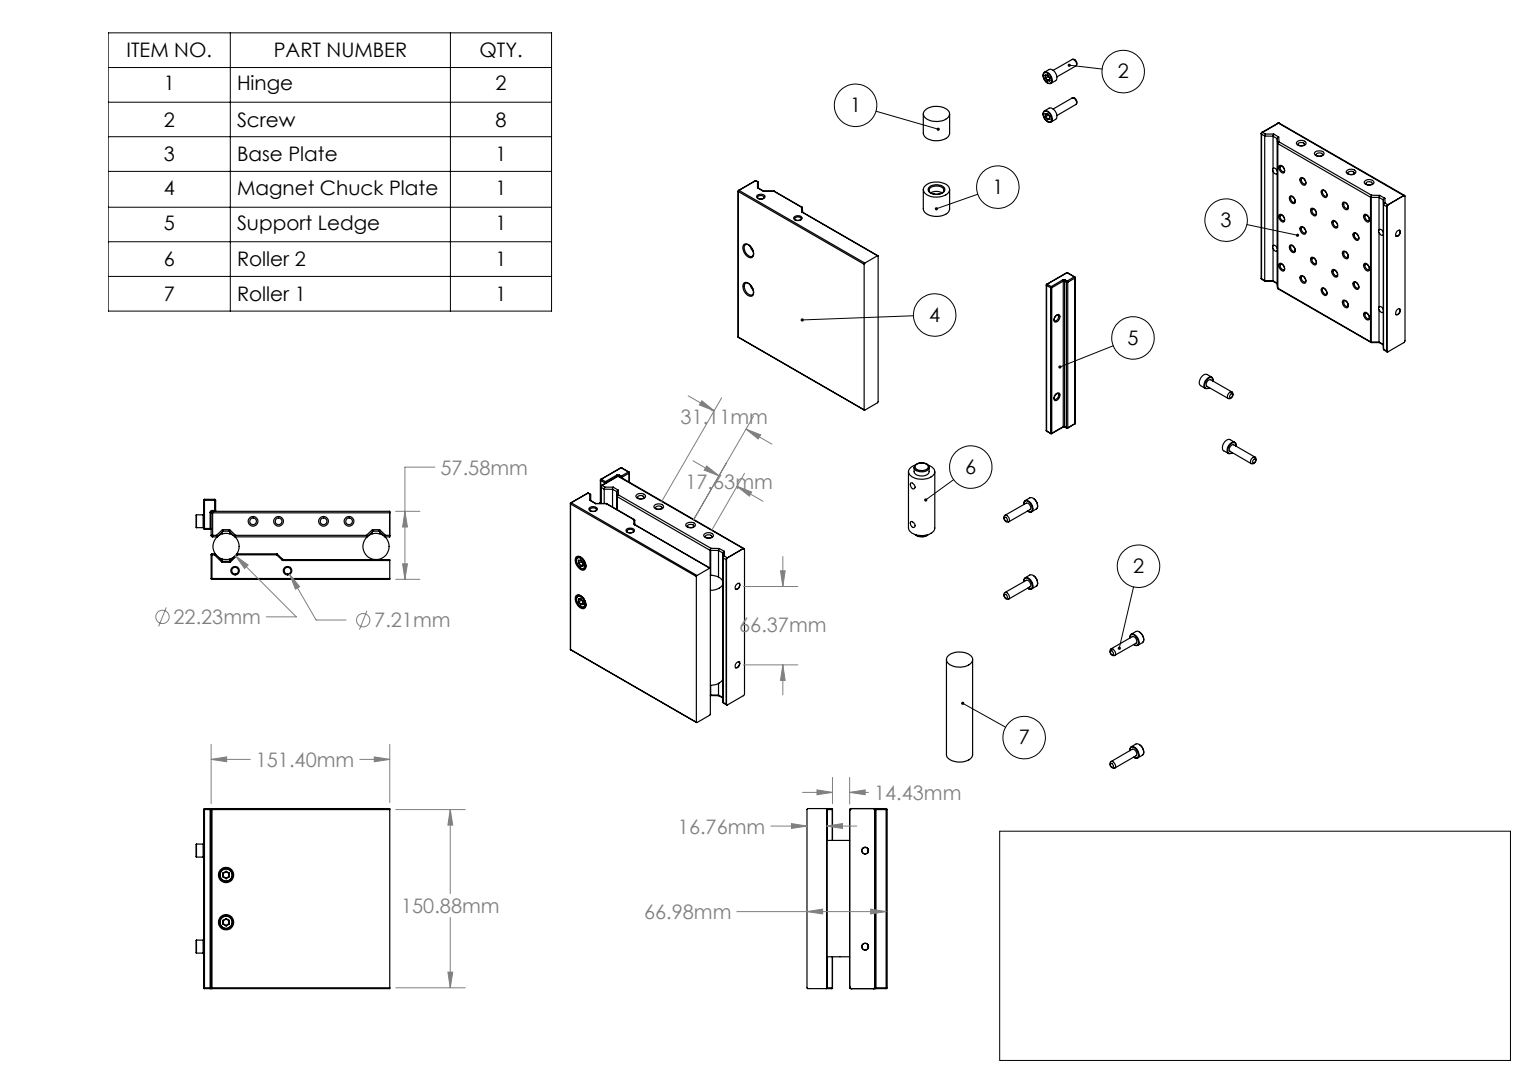
ISO-10303-21;
HEADER;
FILE_DESCRIPTION (('STEP AP214'),
    '1' );
FILE_NAME ('MAT-035',
    '2026-10-26T17:37:43',
    ( '' ),
    ( '' ),
    'SwSTEP 2.0',
    'SolidWorks 2024',
    '' );
FILE_SCHEMA (( 'AUTOMOTIVE_DESIGN' ));
ENDSEC;

DATA;
#1 = EDGE_CURVE ( 'NONE', #5531, #18286, #22565, .T. ) ;
#2 = CARTESIAN_POINT ( 'NONE',  ( 137.0307011298872908, -3580.478779010893959, 2249.731360258177119 ) ) ;
#3 = EDGE_LOOP ( 'NONE', ( #5328, #3633, #22102, #2471 ) ) ;
#4 = DIRECTION ( 'NONE',  ( 0.000000000000000000, 1.000000000000000000, 0.000000000000000000 ) ) ;
#5 = DATE_AND_TIME ( #19692, #20234 ) ;
#6 = CARTESIAN_POINT ( 'NONE',  ( 12.69999999999999929, -3585.971999999999753, 2263.117139999999836 ) ) ;
#7 = CARTESIAN_POINT ( 'NONE',  ( 116.8400000000000034, -3543.299999999999727, 2247.392000000000280 ) ) ;
#8 = VECTOR ( 'NONE', #2227, 1000.000000000000000 ) ;
#9 = DIRECTION ( 'NONE',  ( -1.000000000000000000, 0.000000000000000000, 0.000000000000000000 ) ) ;
#10 = CARTESIAN_POINT ( 'NONE',  ( 0.7620000000000000107, -3544.061999999999898, 2275.763800000000174 ) ) ;
#11 = LOCAL_TIME ( 17, 37, 43.00000000000000000, #12683 ) ;
#12 = CARTESIAN_POINT ( 'NONE',  ( 17.78000000000000114, -3579.494999999999891, 2239.009999999999764 ) ) ;
#13 = EDGE_LOOP ( 'NONE', ( #4801, #14751 ) ) ;
#14 = AXIS2_PLACEMENT_3D ( 'NONE', #15354, #18865, #22602 ) ;
#15 = CARTESIAN_POINT ( 'NONE',  ( 15.55036781974841453, -3695.600514565457615, 2254.996746371283280 ) ) ;
#16 = FACE_OUTER_BOUND ( 'NONE', #5974, .T. ) ;
#17 = ORIENTED_EDGE ( 'NONE', *, *, #15739, .F. ) ;
#18 = CARTESIAN_POINT ( 'NONE',  ( 50.79999999999999716, -3619.500000000000000, 2259.837999999999738 ) ) ;
#19 = LINE ( 'NONE', #12552, #15858 ) ;
#20 = DIRECTION ( 'NONE',  ( 9.756599977372053330E-14, 0.000000000000000000, -1.000000000000000000 ) ) ;
#21 = ORIENTED_EDGE ( 'NONE', *, *, #16592, .T. ) ;
#22 = FACE_OUTER_BOUND ( 'NONE', #22533, .T. ) ;
#23 = DIRECTION ( 'NONE',  ( 0.000000000000000000, 0.000000000000000000, -1.000000000000000000 ) ) ;
#24 = ORIENTED_EDGE ( 'NONE', *, *, #21540, .F. ) ;
#25 = DIRECTION ( 'NONE',  ( 1.000000000000000000, 0.000000000000000000, 3.996303350731721563E-14 ) ) ;
#26 = CARTESIAN_POINT ( 'NONE',  ( 11.76763247656000111, -3642.196447741000156, 2279.779831143999672 ) ) ;
#27 =( NAMED_UNIT ( * ) SI_UNIT ( $, .STERADIAN. ) SOLID_ANGLE_UNIT ( ) );
#28 = SECURITY_CLASSIFICATION ( '', '', #9371 ) ;
#29 = CARTESIAN_POINT ( 'NONE',  ( 17.55427699106284933, -3576.478798487876247, 2245.835327951717773 ) ) ;
#30 = APPLIED_APPROVAL_ASSIGNMENT ( #2619, ( #10933 ) ) ;
#31 = DIRECTION ( 'NONE',  ( 0.000000000000000000, 0.000000000000000000, -1.000000000000000000 ) ) ;
#32 = DATE_AND_TIME ( #21248, #20949 ) ;
#33 = CARTESIAN_POINT ( 'NONE',  ( 139.6999999999999886, -3574.034000000000106, 2239.391000000000076 ) ) ;
#34 = CARTESIAN_POINT ( 'NONE',  ( 9.652920519510999497, -3695.699999999999818, 2254.503999999999905 ) ) ;
#35 = ORIENTED_EDGE ( 'NONE', *, *, #2844, .F. ) ;
#36 = DIRECTION ( 'NONE',  ( 0.000000000000000000, 0.000000000000000000, -1.000000000000000000 ) ) ;
#37 = CARTESIAN_POINT ( 'NONE',  ( 137.2900278743959745, -3657.993505329751770, 2249.258937114173477 ) ) ;
#38 = ORIENTED_EDGE ( 'NONE', *, *, #8360, .F. ) ;
#39 = PLANE ( 'NONE',  #20096 ) ;
#40 = APPLIED_PERSON_AND_ORGANIZATION_ASSIGNMENT ( #1758, #22954, ( #741 ) ) ;
#41 = ORIENTED_EDGE ( 'NONE', *, *, #19227, .F. ) ;
#42 = EDGE_LOOP ( 'NONE', ( #2703, #1001, #9067, #21720 ) ) ;
#43 = SECURITY_CLASSIFICATION ( '', '', #12160 ) ;
#44 = LOCAL_TIME ( 17, 37, 43.00000000000000000, #19509 ) ;
#45 = EDGE_LOOP ( 'NONE', ( #8949, #290, #14111, #10584 ) ) ;
#46 = DIRECTION ( 'NONE',  ( 0.000000000000000000, 0.000000000000000000, -1.000000000000000000 ) ) ;
#47 = EDGE_CURVE ( 'NONE', #7611, #9417, #20192, .T. ) ;
#48 = ORIENTED_EDGE ( 'NONE', *, *, #14973, .T. ) ;
#49 = ORIENTED_EDGE ( 'NONE', *, *, #4852, .F. ) ;
#50 = DIRECTION ( 'NONE',  ( 0.000000000000000000, 0.000000000000000000, -1.000000000000000000 ) ) ;
#51 = ADVANCED_FACE ( 'NONE', ( #16778 ), #19588, .T. ) ;
#52 = APPROVAL_STATUS ( 'not_yet_approved' ) ;
#53 = LINE ( 'NONE', #7432, #17005 ) ;
#54 = CYLINDRICAL_SURFACE ( 'NONE', #7821, 5.714999999999998082 ) ;
#55 = EDGE_CURVE ( 'NONE', #4791, #12834, #15371, .T. ) ;
#56 = EDGE_LOOP ( 'NONE', ( #1910, #7184, #18432, #2575 ) ) ;
#57 = AXIS2_PLACEMENT_3D ( 'NONE', #16806, #751, #19035 ) ;
#58 = CARTESIAN_POINT ( 'NONE',  ( 12.69999999999999929, -3579.494999999999891, 2246.630000000000109 ) ) ;
#59 = CYLINDRICAL_SURFACE ( 'NONE', #10460, 2.844800000000091700 ) ;
#60 = CARTESIAN_POINT ( 'NONE',  ( -12.31900000000000084, -3660.140000000000327, 2247.392000000000280 ) ) ;
#61 = CARTESIAN_POINT ( 'NONE',  ( 116.8400000000000034, -3694.430000000000291, 2247.392000000000280 ) ) ;
#62 = APPROVAL_DATE_TIME ( #1579, #4060 ) ;
#63 = EDGE_CURVE ( 'NONE', #17851, #18027, #1534, .T. ) ;
#64 = DIRECTION ( 'NONE',  ( 0.000000000000000000, -2.336881798971000105E-14, 1.000000000000000000 ) ) ;
#65 = ORIENTED_EDGE ( 'NONE', *, *, #14589, .T. ) ;
#66 = CARTESIAN_POINT ( 'NONE',  ( 9.987313202991684236, -3657.938829547518253, 2239.009999999999764 ) ) ;
#67 = DIRECTION ( 'NONE',  ( 0.000000000000000000, 0.000000000000000000, 1.000000000000000000 ) ) ;
#68 = ORIENTED_EDGE ( 'NONE', *, *, #2483, .T. ) ;
#69 = AXIS2_PLACEMENT_3D ( 'NONE', #21536, #19655, #7123 ) ;
#70 = DIRECTION ( 'NONE',  ( -1.000000000000000000, 2.330758767201999921E-14, 2.343004830739999973E-14 ) ) ;
#71 = CARTESIAN_POINT ( 'NONE',  ( 25.39999999999999858, -3660.140000000000327, 2247.392000000000280 ) ) ;
#72 = CARTESIAN_POINT ( 'NONE',  ( 41.70680000000000121, -3644.899999999999636, 2239.009999999999764 ) ) ;
#73 = CARTESIAN_POINT ( 'NONE',  ( 151.1299999999999955, -3694.430000000000291, 2259.329999999999927 ) ) ;
#74 = DIRECTION ( 'NONE',  ( 0.000000000000000000, 0.000000000000000000, 1.000000000000000000 ) ) ;
#75 = CARTESIAN_POINT ( 'NONE',  ( 18.25500259602790720, -3658.162202898845862, 2245.347138497373180 ) ) ;
#76 = EDGE_CURVE ( 'NONE', #7743, #14640, #1242, .T. ) ;
#77 = EDGE_LOOP ( 'NONE', ( #5442, #11222, #19525, #6801 ) ) ;
#78 = FACE_OUTER_BOUND ( 'NONE', #21782, .T. ) ;
#79 = EDGE_CURVE ( 'NONE', #18611, #6224, #7995, .T. ) ;
#80 = DIRECTION ( 'NONE',  ( 0.000000000000000000, 0.000000000000000000, 1.000000000000000000 ) ) ;
#81 = EDGE_CURVE ( 'NONE', #2498, #2000, #21462, .T. ) ;
#82 = LINE ( 'NONE', #12499, #17173 ) ;
#83 = DIRECTION ( 'NONE',  ( -5.461016542361937364E-28, 1.000000000000000000, -2.336881798971000105E-14 ) ) ;
#84 = CARTESIAN_POINT ( 'NONE',  ( 137.1117535491106594, -3694.976217804482530, 2255.653245237783267 ) ) ;
#85 = ORIENTED_EDGE ( 'NONE', *, *, #8808, .F. ) ;
#86 = AXIS2_PLACEMENT_3D ( 'NONE', #9991, #1078, #11873 ) ;
#87 = DIRECTION ( 'NONE',  ( 0.000000000000000000, 0.000000000000000000, 1.000000000000000000 ) ) ;
#88 = ORIENTED_EDGE ( 'NONE', *, *, #6716, .T. ) ;
#89 = AXIS2_PLACEMENT_3D ( 'NONE', #13714, #3272, #12061 ) ;
#90 = DIRECTION ( 'NONE',  ( 1.000000000000000000, 0.000000000000000000, 0.000000000000000000 ) ) ;
#91 = CARTESIAN_POINT ( 'NONE',  ( 135.0886139726000010, -3662.880847139000252, 2246.630000000000109 ) ) ;
#92 = CALENDAR_DATE ( 2026, 26, 10 ) ;
#93 = CYLINDRICAL_SURFACE ( 'NONE', #6462, 1.269999999999882334 ) ;
#94 = CARTESIAN_POINT ( 'NONE',  ( 3.048000000000000043, -3544.061999999999898, 2228.849999999999909 ) ) ;
#95 = DIRECTION ( 'NONE',  ( -2.336881798971000105E-14, 0.000000000000000000, -1.000000000000000000 ) ) ;
#96 = ADVANCED_FACE ( 'NONE', ( #13964 ), #8465, .F. ) ;
#97 = AXIS2_PLACEMENT_3D ( 'NONE', #21852, #23131, #10839 ) ;
#98 = DIRECTION ( 'NONE',  ( 0.000000000000000000, 0.000000000000000000, 1.000000000000000000 ) ) ;
#99 = AXIS2_PLACEMENT_3D ( 'NONE', #19425, #3130, #10398 ) ;
#100 = ORIENTED_EDGE ( 'NONE', *, *, #20293, .T. ) ;
#101 = DIRECTION ( 'NONE',  ( 0.000000000000000000, 0.000000000000000000, 1.000000000000000000 ) ) ;
#102 = ORIENTED_EDGE ( 'NONE', *, *, #7130, .F. ) ;
#103 = TOROIDAL_SURFACE ( 'NONE', #6096, 3.606799999999999784, 0.7620000000000000107 ) ;
#104 = DIRECTION ( 'NONE',  ( 0.000000000000000000, 0.000000000000000000, -1.000000000000000000 ) ) ;
#105 = CIRCLE ( 'NONE', #22163, 3.606799999999993567 ) ;
#106 = CARTESIAN_POINT ( 'NONE',  ( 139.6999999999999886, -3659.504999999999654, 2272.030000000000200 ) ) ;
#107 = ORIENTED_EDGE ( 'NONE', *, *, #21741, .F. ) ;
#108 = CARTESIAN_POINT ( 'NONE',  ( 85.29320000000001301, -3644.899999999999636, 2239.009999999999764 ) ) ;
#109 = B_SPLINE_CURVE_WITH_KNOTS ( 'NONE', 3,
 ( #11658, #15542, #8166, #2887, #6654, #22328, #18938, #6532, #2998, #1356, #1238, #17171, #20933, #8046, #13430, #10031, #13667, #10147, #3112, #15428, #1118, #2762, #4874, #20571, #12026, #4523, #19295, #6764, #17285, #8277, #9904, #15664, #4637, #20688, #8398, #18816, #19176, #8521, #22561, #22681, #20817, #22437, #17053, #1005, #15312, #6412, #19058, #17399, #13905, #11785, #22788, #21052 ),
 .UNSPECIFIED., .F., .F.,
 ( 4, 2, 1, 1, 1, 1, 2, 2, 2, 1, 2, 2, 2, 2, 1, 1, 1, 2, 2, 2, 2, 1, 1, 1, 2, 2, 2, 1, 1, 1, 2, 2, 4 ),
 ( 0.000000000000000000, 0.003906250000015105105, 0.007812500000030210209, 0.01562500000044777723, 0.03125000000089964147, 0.06250000000180337689, 0.1250000000036391445, 0.2500000000076161855, 0.2656250000084233176, 0.2812500000092305052, 0.3125000000108511533, 0.3750000000142236778, 0.5000000000208256745, 0.5019531250208819628, 0.5039062500209382511, 0.5078125000210353956, 0.5156250000208461026, 0.5312500000204676276, 0.5625000000200504058, 0.6250000000192512672, 0.6289062500191696659, 0.6328125000190880645, 0.6406250000187544424, 0.6562500000179013471, 0.6875000000160184088, 0.7500000000124475985, 0.7539062500122738486, 0.7578125000121000987, 0.7656250000119128041, 0.7812500000113792309, 0.8125000000098967501, 0.8750000000066556760, 1.000000000000000000 ),
 .UNSPECIFIED. ) ;
#110 = EDGE_LOOP ( 'NONE', ( #14632, #871, #3105, #5719 ) ) ;
#111 = CARTESIAN_POINT ( 'NONE',  ( 142.6612001523742208, -3695.684722679518018, 2254.718298691088421 ) ) ;
#112 = DIRECTION ( 'NONE',  ( 1.000000000000000000, 0.000000000000000000, 0.000000000000000000 ) ) ;
#113 = AXIS2_PLACEMENT_3D ( 'NONE', #6268, #9537, #4040 ) ;
#114 = ORIENTED_EDGE ( 'NONE', *, *, #1797, .F. ) ;
#115 = EDGE_CURVE ( 'NONE', #4940, #21098, #2726, .T. ) ;
#116 = ADVANCED_FACE ( 'NONE', ( #12202 ), #6711, .T. ) ;
#117 = CARTESIAN_POINT ( 'NONE',  ( 137.1107034105660034, -3580.676250239197998, 2249.584241783140442 ) ) ;
#118 = VERTEX_POINT ( 'NONE', #15723 ) ;
#119 = DIRECTION ( 'NONE',  ( 1.224646799147353207E-16, 1.000000000000000000, -0.000000000000000000 ) ) ;
#120 = APPLICATION_PROTOCOL_DEFINITION ( 'international standard', 'automotive_design', 2000, #14590 ) ;
#121 = CIRCLE ( 'NONE', #1224, 2.844800000000091700 ) ;
#122 = CARTESIAN_POINT ( 'NONE',  ( 6.996782844457664297, -3579.071241691879095, 2244.547217133379945 ) ) ;
#123 = DIRECTION ( 'NONE',  ( 0.000000000000000000, 0.000000000000000000, -1.000000000000000000 ) ) ;
#124 = ADVANCED_FACE ( 'NONE', ( #19237 ), #13848, .F. ) ;
#125 = DIRECTION ( 'NONE',  ( -1.000000000000000000, 0.000000000000000000, 0.000000000000000000 ) ) ;
#126 = CARTESIAN_POINT ( 'NONE',  ( 12.69999999994000106, -3596.805100000000039, 2292.781800000000203 ) ) ;
#127 = EDGE_LOOP ( 'NONE', ( #9464, #14168, #22567, #17753 ) ) ;
#128 = CARTESIAN_POINT ( 'NONE',  ( 141.9735787716368804, -3577.784544496731542, 2250.025932887172985 ) ) ;
#129 = EDGE_LOOP ( 'NONE', ( #9920, #914 ) ) ;
#130 = AXIS2_PLACEMENT_3D ( 'NONE', #3984, #794, #16512 ) ;
#131 = CARTESIAN_POINT ( 'NONE',  ( 134.0223127011804252, -3578.842640279839998, 2244.547249493357413 ) ) ;
#132 = EDGE_CURVE ( 'NONE', #6511, #15378, #5378, .T. ) ;
#133 = EDGE_CURVE ( 'NONE', #17829, #16978, #3861, .T. ) ;
#134 = CARTESIAN_POINT ( 'NONE',  ( 15.49601198374999989, -3578.946622428999945, 2257.950097350999840 ) ) ;
#135 = ORIENTED_EDGE ( 'NONE', *, *, #969, .F. ) ;
#136 = CARTESIAN_POINT ( 'NONE',  ( 9.970491213060000746, -3580.312548418000006, 2257.932969814999979 ) ) ;
#137 = FACE_OUTER_BOUND ( 'NONE', #12525, .T. ) ;
#138 = CIRCLE ( 'NONE', #3486, 0.7619999999999987894 ) ;
#139 = CLOSED_SHELL ( 'NONE', ( #18289, #7008, #8518, #22594, #20989, #23105, #16145, #3413, #11794, #2224, #2827, #1410, #16543, #19416, #8130, #13424, #4558, #15262, #22286, #8396, #19575, #9289, #13963, #21111, #15810, #7255, #18256, #22413, #19334, #8366, #20531, #3559, #5670, #14740, #18979, #14141, #9599, #14263, #10124, #6147, #22178, #12747, #12264, #9427, #21177, #17826, #16370, #12412, #15426, #5281, #20386, #14683, #16750, #2410, #10013, #13395, #16311, #7711, #4641, #19449, #4494, #20415, #21019, #22225, #51, #6503, #13150, #17175, #14109, #16374, #18246, #13592, #4477, #20450, #11729, #3837, #17376, #8709, #18820, #14659, #4694, #4420, #5580, #11076, #2706, #6139, #12300, #1249, #21474, #5517, #12872, #14173, #13268, #987, #12573, #13097, #1664, #18403, #22007, #19391, #3382, #1211, #5961, #11237, #5886, #6240, #19563, #17791, #16108, #12536, #16780, #15034, #22219, #16319, #12028, #639, #4268, #6646, #19581, #19988, #13241, #6285, #15946, #4264, #21207, #2054, #22523, #7877, #11589, #22115, #16270, #96, #13253, #16398, #4808, #22277, #13435, #22678, #11382, #13308, #16585, #7024, #2755, #9237, #5116, #15881, #12312, #7534, #10663, #16517, #6439, #10126, #19876, #16966, #14807, #20512, #21309, #6853, #805, #16656, #19994, #11360, #8292, #8247, #511, #18141, #8217, #8284, #20809, #15008, #18035, #14102, #15702, #2487, #7663, #10088, #14883, #1165, #15813, #6527, #13028, #17258, #14527, #3507, #2757, #21880, #10849, #8534, #17415, #20660, #18719, #3789, #13015, #1704, #22836, #5727, #9542, #18530, #20029, #22101, #3836, #20839, #5077, #16041, #11870, #14827, #21582, #6419, #5871, #17134, #3910, #5590, #14945, #16186, #7678, #21286, #12539, #7356, #7419, #6403, #1767, #10423, #16431, #5343, #124, #22382, #20876, #14160, #2061, #4392, #471, #2508, #9317, #22720, #967, #22838, #18612, #8833, #5095, #23099, #12516, #18309, #6530, #2705, #20259, #5803, #15689, #10375, #23161, #22806, #22870, #9927, #11310, #13967, #17673, #19716, #15974, #22128, #14003, #5885, #23135, #5290, #5119, #11638, #6284, #7996, #769, #4193, #15853, #18569, #4096, #19675, #3268, #9017, #3364, #233, #11495, #6410, #14763, #6092, #8252, #7227, #12142, #21432 ) ) ;
#140 = VERTEX_POINT ( 'NONE', #15613 ) ;
#141 = DIRECTION ( 'NONE',  ( 1.000000000000000000, 0.000000000000000000, 0.000000000000000000 ) ) ;
#142 = DIRECTION ( 'NONE',  ( 0.000000000000000000, 0.000000000000000000, 1.000000000000000000 ) ) ;
#143 = ORIENTED_EDGE ( 'NONE', *, *, #16586, .F. ) ;
#144 = CARTESIAN_POINT ( 'NONE',  ( -12.69999999999999929, -3577.293829546999859, 2244.679313203000220 ) ) ;
#145 = EDGE_CURVE ( 'NONE', #4963, #5906, #6598, .T. ) ;
#146 = CARTESIAN_POINT ( 'NONE',  ( 139.7000000000063835, -3656.812599999938357, 2239.391000000000076 ) ) ;
#147 = CARTESIAN_POINT ( 'NONE',  ( 86.05520000000001346, -3644.899999999999636, 2261.869999999999891 ) ) ;
#148 = CARTESIAN_POINT ( 'NONE',  ( 35.56000000000000227, -3694.430000000000291, 2243.277199999999993 ) ) ;
#149 = CIRCLE ( 'NONE', #19230, 4.114799999999974034 ) ;
#150 = APPROVAL_ROLE ( '' ) ;
#151 = FACE_OUTER_BOUND ( 'NONE', #1516, .T. ) ;
#152 = CARTESIAN_POINT ( 'NONE',  ( 9.823095770001307514, -3695.626565546511301, 2254.929879519301721 ) ) ;
#153 = EDGE_LOOP ( 'NONE', ( #3229, #589, #13779, #13464, #20523, #7090, #21786, #14841 ) ) ;
#154 = CARTESIAN_POINT ( 'NONE',  ( 18.26408956042804377, -3580.799603742805175, 2245.310931594975045 ) ) ;
#155 = CARTESIAN_POINT ( 'NONE',  ( 137.5777489049088160, -3657.610548859369828, 2248.693836209597066 ) ) ;
#156 = ORIENTED_EDGE ( 'NONE', *, *, #8169, .T. ) ;
#157 = ORIENTED_EDGE ( 'NONE', *, *, #22934, .F. ) ;
#158 = CARTESIAN_POINT ( 'NONE',  ( 137.6199768978073905, -3661.447896576730727, 2249.919485654132586 ) ) ;
#159 = VERTEX_POINT ( 'NONE', #14082 ) ;
#160 = ORIENTED_EDGE ( 'NONE', *, *, #9548, .T. ) ;
#161 = ORIENTED_EDGE ( 'NONE', *, *, #12576, .T. ) ;
#162 = AXIS2_PLACEMENT_3D ( 'NONE', #11218, #12637, #3839 ) ;
#163 = DIRECTION ( 'NONE',  ( 0.000000000000000000, 0.000000000000000000, -1.000000000000000000 ) ) ;
#164 = CIRCLE ( 'NONE', #18872, 1.270000000000000018 ) ;
#165 = ORIENTED_EDGE ( 'NONE', *, *, #16586, .T. ) ;
#166 = ORIENTED_EDGE ( 'NONE', *, *, #22581, .T. ) ;
#167 = DIRECTION ( 'NONE',  ( 1.000000000000000000, -0.000000000000000000, -0.000000000000000000 ) ) ;
#168 = CALENDAR_DATE ( 2026, 26, 10 ) ;
#169 = CARTESIAN_POINT ( 'NONE',  ( 9.956800000000452400, -3660.383257047480583, 2255.967039999999997 ) ) ;
#170 = ORIENTED_EDGE ( 'NONE', *, *, #1350, .F. ) ;
#171 = DIRECTION ( 'NONE',  ( 0.000000000000000000, 1.000000000000000000, 0.000000000000000000 ) ) ;
#172 = CARTESIAN_POINT ( 'NONE',  ( 10.36831320293797276, -3578.148799999986750, 2239.391000000000076 ) ) ;
#173 = PLANE ( 'NONE',  #10602 ) ;
#174 = CARTESIAN_POINT ( 'NONE',  ( -8.890000000008001280, -3580.206200000000081, 2249.723686796999573 ) ) ;
#175 = APPROVAL_DATE_TIME ( #17870, #4630 ) ;
#176 = APPROVAL ( #3017, 'UNKNOWN' ) ;
#177 = CARTESIAN_POINT ( 'NONE',  ( 142.5448000000000093, -3579.495004790000166, 2250.165035197999714 ) ) ;
#178 = EDGE_LOOP ( 'NONE', ( #370, #14088 ) ) ;
#179 = AXIS2_PLACEMENT_3D ( 'NONE', #16153, #101, #7252 ) ;
#180 = AXIS2_PLACEMENT_3D ( 'NONE', #4106, #4219, #18284 ) ;
#181 = CARTESIAN_POINT ( 'NONE',  ( 151.1299999999999955, -3544.570000000000164, 2240.279999999999745 ) ) ;
#182 = EDGE_CURVE ( 'NONE', #17917, #2186, #21094, .T. ) ;
#183 = CARTESIAN_POINT ( 'NONE',  ( 7.963520823585933606, -3662.703639150101026, 2246.156481404430906 ) ) ;
#184 = AXIS2_PLACEMENT_3D ( 'NONE', #20222, #9553, #4165 ) ;
#185 = VERTEX_POINT ( 'NONE', #21235 ) ;
#186 = CARTESIAN_POINT ( 'NONE',  ( 139.6999999999999886, -3659.504999999999654, 2239.391000000000076 ) ) ;
#187 = CARTESIAN_POINT ( 'NONE',  ( 9.987313202740898177, -3661.071170452786646, 2239.009999999999764 ) ) ;
#188 = CARTESIAN_POINT ( 'NONE',  ( 139.6999999999999886, -3579.494999999999891, 2239.009999999999764 ) ) ;
#189 = DIRECTION ( 'NONE',  ( 0.000000000000000000, 1.000000000000000000, 0.000000000000000000 ) ) ;
#190 = ORIENTED_EDGE ( 'NONE', *, *, #21850, .F. ) ;
#191 = CARTESIAN_POINT ( 'NONE',  ( 20.32000000000000028, -3568.700000000000273, 2289.213099999999940 ) ) ;
#192 = EDGE_LOOP ( 'NONE', ( #13601, #391, #20890, #19127 ) ) ;
#193 = CARTESIAN_POINT ( 'NONE',  ( 147.4191677002133929, -3695.185487567203381, 2260.351709085013226 ) ) ;
#194 = AXIS2_PLACEMENT_3D ( 'NONE', #19267, #12347, #20783 ) ;
#195 = CARTESIAN_POINT ( 'NONE',  ( 25.39999999999999858, -3670.300000000000182, 2239.771999999999935 ) ) ;
#196 = AXIS2_PLACEMENT_3D ( 'NONE', #17467, #5408, #21233 ) ;
#197 = DIRECTION ( 'NONE',  ( 0.000000000000000000, 0.000000000000000000, -1.000000000000000000 ) ) ;
#198 = AXIS2_PLACEMENT_3D ( 'NONE', #803, #13353, #20498 ) ;
#199 = DIRECTION ( 'NONE',  ( -1.000000000000000000, -3.885294924352999876E-13, 3.885294924352999876E-13 ) ) ;
#200 = CIRCLE ( 'NONE', #6578, 0.7619999999999294005 ) ;
#201 = DIRECTION ( 'NONE',  ( 0.000000000000000000, 0.000000000000000000, -1.000000000000000000 ) ) ;
#202 = DIRECTION ( 'NONE',  ( 0.000000000000000000, 0.000000000000000000, -1.000000000000000000 ) ) ;
#203 = CARTESIAN_POINT ( 'NONE',  ( 7.471656874357363698, -3577.187248168970200, 2245.090911189840881 ) ) ;
#204 = VERTEX_POINT ( 'NONE', #22501 ) ;
#205 = COORDINATED_UNIVERSAL_TIME_OFFSET ( 0, 0, .AHEAD. ) ;
#206 = APPLIED_PERSON_AND_ORGANIZATION_ASSIGNMENT ( #22202, #11540, ( #4495 ) ) ;
#207 = CARTESIAN_POINT ( 'NONE',  ( -6.349999999999999645, -3578.860000000000127, 2250.998800000000301 ) ) ;
#208 = CARTESIAN_POINT ( 'NONE',  ( 64.76999999999999602, -3544.061999999999898, 2285.606299999999919 ) ) ;
#209 = SECURITY_CLASSIFICATION_LEVEL ( 'unclassified' ) ;
#210 = CARTESIAN_POINT ( 'NONE',  ( 12.69999999999999929, -3599.497499999999945, 2264.841800000000148 ) ) ;
#211 = EDGE_CURVE ( 'NONE', #9937, #6734, #5182, .T. ) ;
#212 = CARTESIAN_POINT ( 'NONE',  ( 127.0000000000000000, -3578.860000000000127, 2247.392000000000280 ) ) ;
#213 = CARTESIAN_POINT ( 'NONE',  ( 88.90000000000000568, -3644.899999999999636, 2239.771999999999935 ) ) ;
#214 = EDGE_CURVE ( 'NONE', #861, #2826, #5753, .T. ) ;
#215 = AXIS2_PLACEMENT_3D ( 'NONE', #7884, #11390, #22164 ) ;
#216 = B_SPLINE_CURVE_WITH_KNOTS ( 'NONE', 3,
 ( #18119, #3820, #429, #5713, #3941, #21530, #9448, #2077, #14847, #4055, #12848, #14381, #19885, #21978, #4168, #5485, #12624, #3704, #7461, #5944, #19777, #18463, #10857, #18005, #1953, #14614, #21868, #12732, #9109, #13074, #20121 ),
 .UNSPECIFIED., .F., .F.,
 ( 4, 2, 2, 2, 2, 2, 1, 2, 2, 2, 2, 1, 1, 2, 2, 2, 4 ),
 ( 0.000000000000000000, 0.1250000000032115977, 0.1875000000050884574, 0.2500000000069653172, 0.3750000000111080589, 0.4375000000130825906, 0.4687500000140698009, 0.4843750000143322576, 0.5000000000145947698, 0.6250000000177098336, 0.6875000000192672545, 0.7187500000200460759, 0.7343750000203067563, 0.7421875000204309902, 0.7500000000205552242, 0.8750000000102775566, 1.000000000000000000 ),
 .UNSPECIFIED. ) ;
#217 = AXIS2_PLACEMENT_3D ( 'NONE', #2919, #10176, #1149 ) ;
#218 = LINE ( 'NONE', #7366, #10755 ) ;
#220 = EDGE_CURVE ( 'NONE', #9973, #10014, #6473, .T. ) ;
#219 = CIRCLE ( 'NONE', #19664, 3.606799999999993567 ) ;
#221 =( REPRESENTATION_RELATIONSHIP ('NONE','NONE', #20448, #13255 ) REPRESENTATION_RELATIONSHIP_WITH_TRANSFORMATION ( #15445 )SHAPE_REPRESENTATION_RELATIONSHIP( ) );
#222 = AXIS2_PLACEMENT_3D ( 'NONE', #21550, #10764, #3608 ) ;
#223 = ORIENTED_EDGE ( 'NONE', *, *, #11710, .T. ) ;
#224 = CARTESIAN_POINT ( 'NONE',  ( 12.69999999999999929, -3579.494999999999891, 2270.760000000000218 ) ) ;
#225 = ORIENTED_EDGE ( 'NONE', *, *, #4542, .T. ) ;
#226 = CARTESIAN_POINT ( 'NONE',  ( 139.6999999999999886, -3659.504999999999654, 2239.771999999999935 ) ) ;
#227 = CARTESIAN_POINT ( 'NONE',  ( 9.855201422231997910, -3639.397391705999780, 2279.447341858000073 ) ) ;
#228 = ORIENTED_EDGE ( 'NONE', *, *, #17836, .F. ) ;
#229 = DIRECTION ( 'NONE',  ( 0.000000000000000000, 0.000000000000000000, -1.000000000000000000 ) ) ;
#230 = ORIENTED_EDGE ( 'NONE', *, *, #20185, .F. ) ;
#231 = DIRECTION ( 'NONE',  ( 0.000000000000000000, 0.000000000000000000, -1.000000000000000000 ) ) ;
#232 = PLANE ( 'NONE',  #19911 ) ;
#233 = ADVANCED_FACE ( 'NONE', ( #17343 ), #7401, .T. ) ;
#234 = AXIS2_PLACEMENT_3D ( 'NONE', #17409, #21062, #21410 ) ;
#235 = VECTOR ( 'NONE', #20474, 1000.000000000000000 ) ;
#236 = EDGE_LOOP ( 'NONE', ( #22169, #11016, #6043, #4841 ) ) ;
#237 = PRODUCT_DEFINITION_SHAPE ( 'NONE', 'NONE',  #17087 ) ;
#238 = AXIS2_PLACEMENT_3D ( 'NONE', #213, #10759, #14515 ) ;
#239 = CARTESIAN_POINT ( 'NONE',  ( 137.7798478441602583, -3581.594086837189934, 2248.178223016279844 ) ) ;
#240 = ORIENTED_EDGE ( 'NONE', *, *, #6122, .T. ) ;
#241 = DIRECTION ( 'NONE',  ( 0.000000000000000000, 1.000000000000000000, 0.000000000000000000 ) ) ;
#242 = AXIS2_PLACEMENT_3D ( 'NONE', #13170, #5587, #11300 ) ;
#243 = APPROVAL_STATUS ( 'not_yet_approved' ) ;
#244 = CIRCLE ( 'NONE', #16685, 5.714999999998999769 ) ;
#245 = CARTESIAN_POINT ( 'NONE',  ( 142.0316867971999955, -3578.148799999999937, 2242.820000000000164 ) ) ;
#246 = FACE_OUTER_BOUND ( 'NONE', #8836, .T. ) ;
#247 = DIRECTION ( 'NONE',  ( -1.000000000000000000, -1.165588477296775430E-12, 0.000000000000000000 ) ) ;
#248 = EDGE_CURVE ( 'NONE', #8112, #12304, #9278, .T. ) ;
#249 = LINE ( 'NONE', #19809, #13213 ) ;
#250 = VECTOR ( 'NONE', #21152, 1000.000000000000000 ) ;
#251 = CARTESIAN_POINT ( 'NONE',  ( 138.0292475174377671, -3577.192411888781862, 2249.696850050126159 ) ) ;
#252 = ORIENTED_EDGE ( 'NONE', *, *, #13501, .F. ) ;
#253 = CARTESIAN_POINT ( 'NONE',  ( 64.76999999999999602, -3543.299999999999727, 2289.213099999999940 ) ) ;
#254 = ADVANCED_FACE ( 'NONE', ( #12432 ), #16297, .F. ) ;
#255 = ADVANCED_FACE ( 'NONE', ( #18168 ), #10909, .F. ) ;
#256 = ORIENTED_EDGE ( 'NONE', *, *, #14397, .F. ) ;
#257 = VERTEX_POINT ( 'NONE', #7279 ) ;
#258 = CARTESIAN_POINT ( 'NONE',  ( 15.39424581079000021, -3598.565999368000121, 2279.486256121999759 ) ) ;
#259 = DIRECTION ( 'NONE',  ( 0.000000000000000000, -1.000000000000000000, 0.000000000000000000 ) ) ;
#260 = AXIS2_PLACEMENT_3D ( 'NONE', #525, #18221, #2401 ) ;
#261 = ORIENTED_EDGE ( 'NONE', *, *, #15365, .F. ) ;
#262 = DIRECTION ( 'NONE',  ( 0.000000000000000000, 0.000000000000000000, -1.000000000000000000 ) ) ;
#263 = DIRECTION ( 'NONE',  ( -2.343004830739999973E-14, -1.784212334590129905E-30, -1.000000000000000000 ) ) ;
#264 = ORIENTED_EDGE ( 'NONE', *, *, #17863, .T. ) ;
#265 = DIRECTION ( 'NONE',  ( 1.000000000000000000, 0.000000000000000000, 0.000000000000000000 ) ) ;
#266 = DIRECTION ( 'NONE',  ( 0.000000000000000000, 0.000000000000000000, -1.000000000000000000 ) ) ;
#267 = DIRECTION ( 'NONE',  ( 1.073225997510925892E-13, 0.000000000000000000, 1.000000000000000000 ) ) ;
#268 = DIRECTION ( 'NONE',  ( -1.000000000000000000, 0.000000000000000000, 0.000000000000000000 ) ) ;
#269 = EDGE_CURVE ( 'NONE', #14110, #7171, #20694, .T. ) ;
#270 = PERSON_AND_ORGANIZATION ( #5446, #1895 ) ;
#271 = ORIENTED_EDGE ( 'NONE', *, *, #4706, .F. ) ;
#272 = CIRCLE ( 'NONE', #10732, 6.477000000000000313 ) ;
#273 = CARTESIAN_POINT ( 'NONE',  ( 20.59150445774999838, -3694.472271328999796, 2260.600000000000364 ) ) ;
#274 = CARTESIAN_POINT ( 'NONE',  ( 9.851025909890511301, -3695.599092773431494, 2255.000090470981831 ) ) ;
#275 = ORIENTED_EDGE ( 'NONE', *, *, #7383, .T. ) ;
#276 = DIRECTION ( 'NONE',  ( -3.561520347316999955E-13, -6.475491540576999783E-13, 1.000000000000000000 ) ) ;
#277 = CIRCLE ( 'NONE', #1377, 5.460999999999938126 ) ;
#278 = CARTESIAN_POINT ( 'NONE',  ( 117.9067999999989951, -3644.899999999999636, 2260.600000000000364 ) ) ;
#279 = VERTEX_POINT ( 'NONE', #21692 ) ;
#280 = CARTESIAN_POINT ( 'NONE',  ( 138.4989950604438604, -3662.085293714453655, 2249.468401061301847 ) ) ;
#281 = EDGE_CURVE ( 'NONE', #13787, #22341, #17933, .T. ) ;
#282 = ORIENTED_EDGE ( 'NONE', *, *, #8857, .F. ) ;
#283 = EDGE_LOOP ( 'NONE', ( #11779, #4580, #14894, #1068 ) ) ;
#284 = CIRCLE ( 'NONE', #2157, 0.7619999999999294005 ) ;
#285 = CARTESIAN_POINT ( 'NONE',  ( 9.916854418464000176, -3578.905956564000007, 2250.236428761999832 ) ) ;
#286 = ORIENTED_EDGE ( 'NONE', *, *, #14831, .T. ) ;
#287 = VERTEX_POINT ( 'NONE', #2127 ) ;
#288 = CARTESIAN_POINT ( 'NONE',  ( 151.4000000000000057, -3694.430000000000291, 2259.329999999999927 ) ) ;
#289 = CARTESIAN_POINT ( 'NONE',  ( -12.69999999999073204, -3658.702685254750122, 2244.902497835748818 ) ) ;
#290 = ORIENTED_EDGE ( 'NONE', *, *, #8429, .F. ) ;
#291 = AXIS2_PLACEMENT_3D ( 'NONE', #23158, #21545, #3370 ) ;
#292 = DIRECTION ( 'NONE',  ( -1.000000000000000000, 2.318894227180000040E-14, 2.343004830739999973E-14 ) ) ;
#293 = CIRCLE ( 'NONE', #11497, 0.7619999999999987894 ) ;
#294 = DIRECTION ( 'NONE',  ( 0.000000000000000000, -1.000000000000000000, 0.000000000000000000 ) ) ;
#295 = DIRECTION ( 'NONE',  ( -9.561467977825806485E-14, 1.000000000000000000, 0.000000000000000000 ) ) ;
#296 = VECTOR ( 'NONE', #22031, 1000.000000000000000 ) ;
#297 = ADVANCED_FACE ( 'NONE', ( #137 ), #12864, .T. ) ;
#298 = APPLICATION_PROTOCOL_DEFINITION ( 'international standard', 'automotive_design', 2000, #1674 ) ;
#299 = EDGE_LOOP ( 'NONE', ( #10110, #17418, #6158, #21329 ) ) ;
#300 = DIRECTION ( 'NONE',  ( -1.000000000000000000, 0.000000000000000000, 0.000000000000000000 ) ) ;
#301 = EDGE_LOOP ( 'NONE', ( #2124, #6129, #13077, #7264 ) ) ;
#302 = DIRECTION ( 'NONE',  ( 2.336881798971000105E-14, 0.000000000000000000, 1.000000000000000000 ) ) ;
#303 = DIRECTION ( 'NONE',  ( -1.000000000000000000, 1.224646799147353207E-16, 0.000000000000000000 ) ) ;
#304 = CARTESIAN_POINT ( 'NONE',  ( 1.270000000000000018, -3578.860000000000127, 2244.547199999999975 ) ) ;
#305 = ORIENTED_EDGE ( 'NONE', *, *, #9304, .F. ) ;
#306 = CARTESIAN_POINT ( 'NONE',  ( 95.25000000000000000, -3544.570000000000164, 2247.392000000000280 ) ) ;
#307 = CARTESIAN_POINT ( 'NONE',  ( 63.50000000000000000, -3594.099999999999909, 2259.837999999999738 ) ) ;
#308 = CARTESIAN_POINT ( 'NONE',  ( 139.6999999999999886, -3579.494999999999891, 2270.760000000000218 ) ) ;
#309 = VERTEX_POINT ( 'NONE', #12898 ) ;
#310 = CARTESIAN_POINT ( 'NONE',  ( 18.11219821918659179, -3657.669286988329986, 2245.981668378579798 ) ) ;
#311 = ORIENTED_EDGE ( 'NONE', *, *, #22098, .F. ) ;
#312 = DIRECTION ( 'NONE',  ( -1.000000000000000000, 0.000000000000000000, 0.000000000000000000 ) ) ;
#313 = DIRECTION ( 'NONE',  ( -1.000000000000000000, 0.000000000000000000, 0.000000000000000000 ) ) ;
#314 = DIRECTION ( 'NONE',  ( 0.000000000000000000, -1.000000000000000000, 0.000000000000000000 ) ) ;
#315 = TOROIDAL_SURFACE ( 'NONE', #12233, 3.606799999999999784, 0.7620000000000000107 ) ;
#316 = CARTESIAN_POINT ( 'NONE',  ( 142.5448000000000093, -3579.495004790000166, 2250.165035197999714 ) ) ;
#317 = FACE_OUTER_BOUND ( 'NONE', #5413, .T. ) ;
#318 = CARTESIAN_POINT ( 'NONE',  ( 137.0608322996959316, -3695.185487567919154, 2255.525709084477512 ) ) ;
#319 = CARTESIAN_POINT ( 'NONE',  ( 7.834922896206100162, -3576.496315022116505, 2245.808993730167458 ) ) ;
#320 = ORIENTED_EDGE ( 'NONE', *, *, #15713, .T. ) ;
#321 = COORDINATED_UNIVERSAL_TIME_OFFSET ( 0, 0, .AHEAD. ) ;
#322 = CARTESIAN_POINT ( 'NONE',  ( -12.69999999999997442, -3657.007659094873816, 2247.391999999781547 ) ) ;
#323 = DIRECTION ( 'NONE',  ( 0.000000000000000000, -1.000000000000000000, 0.000000000000000000 ) ) ;
#324 = CARTESIAN_POINT ( 'NONE',  ( 12.70000000000000107, -3570.287499999999909, 2279.817639999999756 ) ) ;
#325 = CARTESIAN_POINT ( 'NONE',  ( 29.00679999999900005, -3619.500000000000000, 2239.771999999999935 ) ) ;
#326 = FACE_OUTER_BOUND ( 'NONE', #6088, .T. ) ;
#327 = ORIENTED_EDGE ( 'NONE', *, *, #11023, .F. ) ;
#328 = DIRECTION ( 'NONE',  ( 1.000000000000000000, 0.000000000000000000, 0.000000000000000000 ) ) ;
#329 = EDGE_LOOP ( 'NONE', ( #8854, #6013, #22023, #18423, #7464, #6906 ) ) ;
#330 = CIRCLE ( 'NONE', #16415, 0.7619999999999294005 ) ;
#331 = CARTESIAN_POINT ( 'NONE',  ( 47.19319999999999737, -3670.300000000000182, 2260.600000000000364 ) ) ;
#332 = APPLIED_PERSON_AND_ORGANIZATION_ASSIGNMENT ( #8359, #9988, ( #10138 ) ) ;
#333 = EDGE_CURVE ( 'NONE', #1510, #18918, #3750, .T. ) ;
#334 = CARTESIAN_POINT ( 'NONE',  ( 12.69997783158000004, -3636.657698770999559, 2279.817639764999967 ) ) ;
#335 = ORIENTED_EDGE ( 'NONE', *, *, #8776, .F. ) ;
#336 = FACE_OUTER_BOUND ( 'NONE', #5464, .T. ) ;
#337 = EDGE_CURVE ( 'NONE', #11629, #10297, #6048, .T. ) ;
#338 = ORIENTED_EDGE ( 'NONE', *, *, #15407, .T. ) ;
#339 = DIRECTION ( 'NONE',  ( 0.000000000000000000, -1.165588477296860248E-12, 1.000000000000000000 ) ) ;
#340 = DIRECTION ( 'NONE',  ( 1.000000000000000000, 0.000000000000000000, 0.000000000000000000 ) ) ;
#341 = EDGE_CURVE ( 'NONE', #9417, #7352, #19, .T. ) ;
#342 = ORIENTED_EDGE ( 'NONE', *, *, #3117, .T. ) ;
#343 = EDGE_CURVE ( 'NONE', #1907, #13051, #5539, .T. ) ;
#344 = CARTESIAN_POINT ( 'NONE',  ( 137.7661303793067873, -3581.581515421061795, 2248.220692510852587 ) ) ;
#345 = PRODUCT_DEFINITION_CONTEXT ( 'detailed design', #1225, 'design' ) ;
#346 = ORIENTED_EDGE ( 'NONE', *, *, #18787, .T. ) ;
#347 = AXIS2_PLACEMENT_3D ( 'NONE', #19188, #3123, #5242 ) ;
#348 = DIRECTION ( 'NONE',  ( 0.000000000000000000, 0.000000000000000000, 1.000000000000000000 ) ) ;
#349 = APPROVAL_ROLE ( '' ) ;
#350 = CARTESIAN_POINT ( 'NONE',  ( 15.39424449907000003, -3640.434004351000112, 2279.486256451000372 ) ) ;
#351 = EDGE_CURVE ( 'NONE', #22087, #15975, #10618, .T. ) ;
#352 = CARTESIAN_POINT ( 'NONE',  ( 1.270000000000000018, -3694.430000000000291, 2240.279999999999745 ) ) ;
#353 = CARTESIAN_POINT ( 'NONE',  ( 133.9849999999989905, -3579.494999999999891, 2239.771999999999935 ) ) ;
#354 = CARTESIAN_POINT ( 'NONE',  ( 10.36831320289401859, -3640.848700000111421, 2296.210799999999836 ) ) ;
#355 = ADVANCED_FACE ( 'NONE', ( #3996 ), #10792, .T. ) ;
#356 = CARTESIAN_POINT ( 'NONE',  ( 138.7293422311318807, -3576.819596326436567, 2249.374802684401402 ) ) ;
#357 = ORIENTED_EDGE ( 'NONE', *, *, #14314, .T. ) ;
#358 = DIRECTION ( 'NONE',  ( 0.000000000000000000, 0.000000000000000000, 1.000000000000000000 ) ) ;
#359 = AXIS2_PLACEMENT_3D ( 'NONE', #17047, #1111, #22432 ) ;
#360 = DIRECTION ( 'NONE',  ( 0.000000000000000000, 0.000000000000000000, 1.000000000000000000 ) ) ;
#361 = ORIENTED_EDGE ( 'NONE', *, *, #15519, .F. ) ;
#362 = CARTESIAN_POINT ( 'NONE',  ( 6.985000000000000320, -3659.504999999999654, 2239.771999999999935 ) ) ;
#363 = AXIS2_PLACEMENT_3D ( 'NONE', #2504, #11180, #9647 ) ;
#364 = DIRECTION ( 'NONE',  ( 1.298916404569000195E-12, -1.000000000000000000, 0.000000000000000000 ) ) ;
#365 = ORIENTED_EDGE ( 'NONE', *, *, #11427, .T. ) ;
#366 = CARTESIAN_POINT ( 'NONE',  ( 14.03509158661000100, -3662.022285901000032, 2257.672186979000344 ) ) ;
#367 = EDGE_CURVE ( 'NONE', #20138, #17884, #3501, .T. ) ;
#368 = DIRECTION ( 'NONE',  ( 0.000000000000000000, 0.000000000000000000, -1.000000000000000000 ) ) ;
#369 = EDGE_CURVE ( 'NONE', #923, #11706, #14203, .T. ) ;
#370 = ORIENTED_EDGE ( 'NONE', *, *, #1712, .T. ) ;
#371 = EDGE_CURVE ( 'NONE', #830, #1510, #5294, .T. ) ;
#372 = CYLINDRICAL_SURFACE ( 'NONE', #653, 1.269999999999882334 ) ;
#373 = DIRECTION ( 'NONE',  ( 0.000000000000000000, 0.000000000000000000, 1.000000000000000000 ) ) ;
#374 = DIRECTION ( 'NONE',  ( 0.000000000000000000, 0.000000000000000000, -1.000000000000000000 ) ) ;
#375 = ORIENTED_EDGE ( 'NONE', *, *, #3846, .F. ) ;
#376 = DIRECTION ( 'NONE',  ( 1.000000000000000000, 5.432398939370943590E-28, -2.324635735433000369E-14 ) ) ;
#377 = APPROVAL_ROLE ( '' ) ;
#378 = DIRECTION ( 'NONE',  ( 1.000000000000000000, -0.000000000000000000, 1.224646799147353207E-16 ) ) ;
#379 = DIRECTION ( 'NONE',  ( 0.8068916933307923589, -0.5906994119124941989, 0.000000000000000000 ) ) ;
#380 = ORIENTED_EDGE ( 'NONE', *, *, #14174, .F. ) ;
#381 = SECURITY_CLASSIFICATION ( '', '', #20645 ) ;
#382 = CARTESIAN_POINT ( 'NONE',  ( 18.14049516396890027, -3581.245129373504369, 2245.841260512669123 ) ) ;
#383 = DIRECTION ( 'NONE',  ( -1.000000000000000000, 2.330758767201999921E-14, 2.356218894535000080E-14 ) ) ;
#384 = ADVANCED_FACE ( 'NONE', ( #14318 ), #1776, .F. ) ;
#385 = EDGE_LOOP ( 'NONE', ( #5161, #4058, #19864, #16959, #15147, #3031 ) ) ;
#386 = CARTESIAN_POINT ( 'NONE',  ( 138.2628149773561290, -3661.960543573507948, 2249.578175895470395 ) ) ;
#387 = ORIENTED_EDGE ( 'NONE', *, *, #4635, .F. ) ;
#388 = ORIENTED_EDGE ( 'NONE', *, *, #4639, .T. ) ;
#389 = AXIS2_PLACEMENT_3D ( 'NONE', #3368, #21197, #5143 ) ;
#390 = CARTESIAN_POINT ( 'NONE',  ( 12.69999999994000106, -3636.810100000000148, 2296.210799999999836 ) ) ;
#391 = ORIENTED_EDGE ( 'NONE', *, *, #20683, .T. ) ;
#392 = ORIENTED_EDGE ( 'NONE', *, *, #12214, .T. ) ;
#393 = APPLIED_APPROVAL_ASSIGNMENT ( #3604, ( #741 ) ) ;
#394 = DIRECTION ( 'NONE',  ( -1.000000000000000000, 0.000000000000000000, 0.000000000000000000 ) ) ;
#395 = FACE_OUTER_BOUND ( 'NONE', #15654, .T. ) ;
#396 = LOCAL_TIME ( 17, 37, 43.00000000000000000, #13422 ) ;
#397 = ORIENTED_EDGE ( 'NONE', *, *, #13639, .F. ) ;
#398 = FACE_OUTER_BOUND ( 'NONE', #16979, .T. ) ;
#399 = CARTESIAN_POINT ( 'NONE',  ( 7.254607931487381478, -3581.231065619790570, 2245.814675045431159 ) ) ;
#400 = CARTESIAN_POINT ( 'NONE',  ( 19.17699999999999960, -3639.502500000000055, 2295.829799999999977 ) ) ;
#401 = APPROVAL_DATE_TIME ( #11400, #11350 ) ;
#402 = EDGE_CURVE ( 'NONE', #14892, #830, #14431, .T. ) ;
#403 = DIRECTION ( 'NONE',  ( 1.000000000000000000, 0.000000000000000000, 0.000000000000000000 ) ) ;
#404 = EDGE_CURVE ( 'NONE', #2635, #21912, #17488, .T. ) ;
#405 = ORIENTED_EDGE ( 'NONE', *, *, #418, .F. ) ;
#406 = DIRECTION ( 'NONE',  ( 0.000000000000000000, -0.8660254037825031448, -0.5000000000033524294 ) ) ;
#407 = DIRECTION ( 'NONE',  ( 0.000000000000000000, 1.000000000000000000, 0.000000000000000000 ) ) ;
#408 = APPLIED_APPROVAL_ASSIGNMENT ( #14062, ( #20600 ) ) ;
#409 = EDGE_CURVE ( 'NONE', #2915, #8062, #11888, .T. ) ;
#410 = LOCAL_TIME ( 17, 37, 43.00000000000000000, #12824 ) ;
#411 = DIRECTION ( 'NONE',  ( -2.356218894535439317E-14, 0.000000000000000000, -1.000000000000000000 ) ) ;
#412 = ORIENTED_EDGE ( 'NONE', *, *, #21540, .T. ) ;
#413 = DIRECTION ( 'NONE',  ( 1.000000000000000000, 0.000000000000000000, 0.000000000000000000 ) ) ;
#414 = CIRCLE ( 'NONE', #13497, 3.606800000000021100 ) ;
#415 = LINE ( 'NONE', #12612, #10639 ) ;
#416 = ADVANCED_BREP_SHAPE_REPRESENTATION ( '', ( #13560, #5611 ), #2257 ) ;
#417 = DIRECTION ( 'NONE',  ( 0.000000000000000000, 0.000000000000000000, -1.000000000000000000 ) ) ;
#418 = EDGE_CURVE ( 'NONE', #21665, #9059, #5768, .T. ) ;
#419 = DIRECTION ( 'NONE',  ( 0.000000000000000000, 1.000000000000000000, 0.000000000000000000 ) ) ;
#420 = ORIENTED_EDGE ( 'NONE', *, *, #341, .F. ) ;
#421 = AXIS2_PLACEMENT_3D ( 'NONE', #17372, #1683, #23118 ) ;
#422 = ADVANCED_FACE ( 'NONE', ( #15004 ), #20281, .T. ) ;
#423 = CARTESIAN_POINT ( 'NONE',  ( 147.6218463403696433, -3543.408637598981386, 2259.843959195220123 ) ) ;
#424 = VERTEX_POINT ( 'NONE', #18285 ) ;
#425 = CARTESIAN_POINT ( 'NONE',  ( 147.5078116312014060, -3695.420022018752661, 2260.129812754224076 ) ) ;
#426 = DIRECTION ( 'NONE',  ( 0.000000000000000000, 0.000000000000000000, 1.000000000000000000 ) ) ;
#427 = DIRECTION ( 'NONE',  ( 1.000000000000000000, 0.000000000000000000, 0.000000000000000000 ) ) ;
#428 = DIRECTION ( 'NONE',  ( 1.000000000000000000, 0.000000000000000000, 0.000000000000000000 ) ) ;
#429 = CARTESIAN_POINT ( 'NONE',  ( 142.2430419228115284, -3544.409801990574579, 2255.766443268943476 ) ) ;
#430 = CARTESIAN_POINT ( 'NONE',  ( 12.69999999999999929, -3659.504999999999654, 2239.391000000000076 ) ) ;
#431 = DIRECTION ( 'NONE',  ( 1.985099921814000023E-12, 1.000000000000000000, 3.793660610075000646E-12 ) ) ;
#432 = EDGE_LOOP ( 'NONE', ( #3093, #2763, #22698, #4638, #1822, #2216, #11281, #2261, #21042, #12609, #19289, #12841, #4089, #6399 ) ) ;
#433 = APPROVAL_STATUS ( 'not_yet_approved' ) ;
#434 = EDGE_CURVE ( 'NONE', #17725, #22994, #2393, .T. ) ;
#435 = CARTESIAN_POINT ( 'NONE',  ( -12.69999999999999929, -3661.706170453011509, 2250.104686796980332 ) ) ;
#436 = DIRECTION ( 'NONE',  ( 0.000000000000000000, 0.000000000000000000, -1.000000000000000000 ) ) ;
#437 = CIRCLE ( 'NONE', #19133, 0.7619999999999987894 ) ;
#438 = VECTOR ( 'NONE', #18888, 1000.000000000000000 ) ;
#439 = DIRECTION ( 'NONE',  ( 0.000000000000000000, 0.000000000000000000, -1.000000000000000000 ) ) ;
#440 = DIRECTION ( 'NONE',  ( 1.000000000000000000, 0.000000000000000000, 0.000000000000000000 ) ) ;
#441 = CARTESIAN_POINT ( 'NONE',  ( 55.57575231171000496, -3544.061999999999898, 2275.763800000000174 ) ) ;
#442 = ORIENTED_EDGE ( 'NONE', *, *, #1926, .T. ) ;
#443 = CARTESIAN_POINT ( 'NONE',  ( 10.36831320285999958, -3658.158799999999701, 2242.820000000000164 ) ) ;
#444 = VERTEX_POINT ( 'NONE', #17555 ) ;
#445 = CARTESIAN_POINT ( 'NONE',  ( 50.79999999999999716, -3568.700000000000273, 2259.837999999999738 ) ) ;
#446 = DIRECTION ( 'NONE',  ( 0.000000000000000000, 0.000000000000000000, -1.000000000000000000 ) ) ;
#447 = ORIENTED_EDGE ( 'NONE', *, *, #18326, .F. ) ;
#448 = FACE_OUTER_BOUND ( 'NONE', #9717, .T. ) ;
#449 = CIRCLE ( 'NONE', #16159, 1.269999999999882334 ) ;
#450 = LINE ( 'NONE', #16612, #19312 ) ;
#451 = AXIS2_PLACEMENT_3D ( 'NONE', #16867, #16981, #7976 ) ;
#452 = VERTEX_POINT ( 'NONE', #1504 ) ;
#453 = DIRECTION ( 'NONE',  ( -1.000000000000000000, -0.000000000000000000, -0.000000000000000000 ) ) ;
#454 = DIRECTION ( 'NONE',  ( -1.224646799147353207E-16, 1.000000000000000000, 0.000000000000000000 ) ) ;
#455 = EDGE_LOOP ( 'NONE', ( #21081, #11505 ) ) ;
#456 = CARTESIAN_POINT ( 'NONE',  ( 137.9046276598544978, -3581.701726360760404, 2247.546642836707633 ) ) ;
#457 = ORIENTED_EDGE ( 'NONE', *, *, #13685, .F. ) ;
#458 = CARTESIAN_POINT ( 'NONE',  ( 145.3734778515583344, -3580.182493284074553, 2244.873281192526065 ) ) ;
#460 = TOROIDAL_SURFACE ( 'NONE', #16565, 6.476999999999000224, 0.7620000000000000107 ) ;
#459 = ITEM_DEFINED_TRANSFORMATION ( 'NONE', 'NONE', #8609,  #5611 ) ;
#461 = APPLIED_DATE_AND_TIME_ASSIGNMENT ( #10547, #22837, ( #22928 ) ) ;
#462 = CARTESIAN_POINT ( 'NONE',  ( 15.27310817925000030, -3640.729796071000237, 2279.515941249000207 ) ) ;
#463 = DIRECTION ( 'NONE',  ( -0.8660254037840939834, -0.5000000000005969669, 0.000000000000000000 ) ) ;
#464 = AXIS2_PLACEMENT_3D ( 'NONE', #19542, #12397, #1487 ) ;
#465 = CARTESIAN_POINT ( 'NONE',  ( 25.39999999999999858, -3660.140000000000327, 2244.547199999999975 ) ) ;
#466 = CARTESIAN_POINT ( 'NONE',  ( 145.4149999980000132, -3659.715610845466017, 2244.570779584676529 ) ) ;
#467 = VECTOR ( 'NONE', #18120, 1000.000000000000000 ) ;
#468 = EDGE_CURVE ( 'NONE', #10446, #7103, #4622, .T. ) ;
#469 = CARTESIAN_POINT ( 'NONE',  ( 141.6187116912652186, -3577.394048819144245, 2249.830271027571598 ) ) ;
#470 = ORIENTED_EDGE ( 'NONE', *, *, #12681, .F. ) ;
#471 = ADVANCED_FACE ( 'NONE', ( #6567 ), #18840, .T. ) ;
#472 = CARTESIAN_POINT ( 'NONE',  ( -5.588000000000000078, -3694.938000000000102, 2253.487999999999829 ) ) ;
#473 = VERTEX_POINT ( 'NONE', #13826 ) ;
#474 = DIRECTION ( 'NONE',  ( 0.000000000000000000, -1.000000000000000000, 0.000000000000000000 ) ) ;
#475 = CARTESIAN_POINT ( 'NONE',  ( 15.54870723730916104, -3543.401189131915999, 2255.000759462869155 ) ) ;
#476 = AXIS2_PLACEMENT_3D ( 'NONE', #15163, #22181, #14935 ) ;
#477 = ORIENTED_EDGE ( 'NONE', *, *, #20451, .T. ) ;
#478 = CARTESIAN_POINT ( 'NONE',  ( 127.0000000000000000, -3568.700000000000273, 2239.771999999999935 ) ) ;
#479 = CARTESIAN_POINT ( 'NONE',  ( 9.855201422231997910, -3599.392391706000126, 2279.447341858000073 ) ) ;
#480 = AXIS2_PLACEMENT_3D ( 'NONE', #16637, #2358, #16527 ) ;
#481 = ORIENTED_EDGE ( 'NONE', *, *, #20058, .F. ) ;
#482 = AXIS2_PLACEMENT_3D ( 'NONE', #17591, #1542, #8584 ) ;
#483 = APPLICATION_CONTEXT ( 'configuration controlled 3d designs of mechanical parts and assemblies' ) ;
#484 = DIRECTION ( 'NONE',  ( 0.000000000000000000, 1.000000000000000000, 0.000000000000000000 ) ) ;
#485 = CARTESIAN_POINT ( 'NONE',  ( 13.71111753102643327, -3576.835601115875306, 2249.390789936909187 ) ) ;
#486 = DIRECTION ( 'NONE',  ( 1.000000000000000000, 0.000000000000000000, 0.000000000000000000 ) ) ;
#487 = DIRECTION ( 'NONE',  ( 0.000000000000000000, 0.000000000000000000, -1.000000000000000000 ) ) ;
#488 = ORIENTED_EDGE ( 'NONE', *, *, #7154, .F. ) ;
#489 = DIRECTION ( 'NONE',  ( 0.000000000000000000, -1.000000000000000000, 0.000000000000000000 ) ) ;
#490 = PERSON_AND_ORGANIZATION ( #5446, #1895 ) ;
#491 = APPLIED_DATE_AND_TIME_ASSIGNMENT ( #13189, #4291, ( #3761 ) ) ;
#492 = CARTESIAN_POINT ( 'NONE',  ( 22.54063073453000143, -3695.699999999999818, 2275.763800000000174 ) ) ;
#493 = FACE_OUTER_BOUND ( 'NONE', #11392, .T. ) ;
#494 = ORIENTED_EDGE ( 'NONE', *, *, #11128, .T. ) ;
#495 = CARTESIAN_POINT ( 'NONE',  ( 18.12359179772333206, -3581.296656515060022, 2245.923799407296883 ) ) ;
#496 = AXIS2_PLACEMENT_3D ( 'NONE', #13817, #20958, #9934 ) ;
#497 = CARTESIAN_POINT ( 'NONE',  ( 138.7804567094461561, -3576.796478203516017, 2257.629402114759159 ) ) ;
#498 = ADVANCED_FACE ( 'NONE', ( #17092 ), #10062, .T. ) ;
#499 = ORIENTED_EDGE ( 'NONE', *, *, #7556, .F. ) ;
#500 = CIRCLE ( 'NONE', #22927, 3.606800000000000228 ) ;
#501 = EDGE_CURVE ( 'NONE', #14295, #9663, #683, .T. ) ;
#502 = CARTESIAN_POINT ( 'NONE',  ( 141.3123101578824787, -3661.849600747001659, 2249.666225506271530 ) ) ;
#503 = EDGE_CURVE ( 'NONE', #4557, #452, #5825, .T. ) ;
#504 = AXIS2_PLACEMENT_3D ( 'NONE', #7643, #14804, #7882 ) ;
#505 = ORIENTED_EDGE ( 'NONE', *, *, #11069, .T. ) ;
#506 = ORIENTED_EDGE ( 'NONE', *, *, #6294, .F. ) ;
#507 = DIRECTION ( 'NONE',  ( -1.000000000000000000, 0.000000000000000000, 0.000000000000000000 ) ) ;
#508 = ORIENTED_EDGE ( 'NONE', *, *, #16803, .F. ) ;
#509 = FACE_OUTER_BOUND ( 'NONE', #5261, .T. ) ;
#510 = CARTESIAN_POINT ( 'NONE',  ( 61.26424768829000556, -3695.699999999999818, 2280.589800000000196 ) ) ;
#511 = ADVANCED_FACE ( 'NONE', ( #11306 ), #18000, .F. ) ;
#512 = CIRCLE ( 'NONE', #14369, 0.3809999999999647002 ) ;
#513 = ORIENTED_EDGE ( 'NONE', *, *, #7023, .T. ) ;
#514 = CARTESIAN_POINT ( 'NONE',  ( 6.985153502415998972, -3659.391482155004724, 2244.644944835688875 ) ) ;
#515 = CARTESIAN_POINT ( 'NONE',  ( 7.283171614331794608, -3581.316932381231254, 2245.957881525527227 ) ) ;
#516 = EDGE_CURVE ( 'NONE', #8087, #21408, #6409, .T. ) ;
#517 = DIRECTION ( 'NONE',  ( -1.000000000000000000, 0.000000000000000000, 3.885294924357999613E-13 ) ) ;
#518 = DATE_AND_TIME ( #5921, #1865 ) ;
#519 = VECTOR ( 'NONE', #3642, 1000.000000000000000 ) ;
#520 = LINE ( 'NONE', #7549, #8680 ) ;
#521 = CARTESIAN_POINT ( 'NONE',  ( 76.20000000000000284, -3670.300000000000182, 2259.837999999999738 ) ) ;
#522 = DIRECTION ( 'NONE',  ( 0.000000000000000000, 0.000000000000000000, 1.000000000000000000 ) ) ;
#523 = VERTEX_POINT ( 'NONE', #18112 ) ;
#524 = AXIS2_PLACEMENT_3D ( 'NONE', #11468, #8077, #15225 ) ;
#525 = CARTESIAN_POINT ( 'NONE',  ( 15.24000000000000021, -3695.699999999999818, 2255.774000000000342 ) ) ;
#526 = EDGE_CURVE ( 'NONE', #16634, #17242, #1905, .T. ) ;
#527 = DIRECTION ( 'NONE',  ( 0.000000000000000000, -1.000000000000000000, 0.000000000000000000 ) ) ;
#528 = FACE_OUTER_BOUND ( 'NONE', #10890, .T. ) ;
#529 = DIRECTION ( 'NONE',  ( 0.000000000000000000, 2.336881798971000105E-14, -1.000000000000000000 ) ) ;
#530 = ADVANCED_FACE ( 'NONE', ( #9101 ), #16243, .F. ) ;
#531 = EDGE_CURVE ( 'NONE', #3180, #17789, #10470, .T. ) ;
#532 = DIRECTION ( 'NONE',  ( 0.000000000000000000, 0.000000000000000000, -1.000000000000000000 ) ) ;
#533 = ORIENTED_EDGE ( 'NONE', *, *, #21014, .F. ) ;
#534 = CARTESIAN_POINT ( 'NONE',  ( 15.54479972196000048, -3659.504990611520043, 2257.962943248000101 ) ) ;
#535 = DIRECTION ( 'NONE',  ( 0.000000000000000000, 0.000000000000000000, 1.000000000000000000 ) ) ;
#536 = SHAPE_REPRESENTATION ( 'Screw 7', ( #5611 ), #5641 ) ;
#537 = DIRECTION ( 'NONE',  ( 1.000000000000000000, -0.000000000000000000, 1.224646799147353207E-16 ) ) ;
#538 = CARTESIAN_POINT ( 'NONE',  ( -6.730999999999999872, -3660.140000000000327, 2247.392000000000280 ) ) ;
#539 = CYLINDRICAL_SURFACE ( 'NONE', #15070, 2.844799999998995244 ) ;
#540 = DIRECTION ( 'NONE',  ( 0.8660254037824132167, -0.5000000000035080827, -5.278136500991081487E-12 ) ) ;
#541 = CIRCLE ( 'NONE', #4305, 2.844800000000091700 ) ;
#542 = LINE ( 'NONE', #21648, #18834 ) ;
#543 = ORIENTED_EDGE ( 'NONE', *, *, #6594, .F. ) ;
#544 = COORDINATED_UNIVERSAL_TIME_OFFSET ( 0, 0, .AHEAD. ) ;
#545 = AXIS2_PLACEMENT_3D ( 'NONE', #4764, #11911, #21519 ) ;
#546 = VECTOR ( 'NONE', #10969, 1000.000000000000114 ) ;
#547 = CARTESIAN_POINT ( 'NONE',  ( 145.4149999978999972, -3659.505243078000149, 2244.618209833000492 ) ) ;
#548 = EDGE_CURVE ( 'NONE', #6059, #12867, #16146, .T. ) ;
#549 = CARTESIAN_POINT ( 'NONE',  ( 10.01629450381963693, -3580.440293654210564, 2249.758428457885657 ) ) ;
#550 = CARTESIAN_POINT ( 'NONE',  ( 38.10000000000000142, -3594.099999999999909, 2261.869999999999891 ) ) ;
#551 = EDGE_LOOP ( 'NONE', ( #13315, #19240, #6873, #12519 ) ) ;
#552 = FACE_OUTER_BOUND ( 'NONE', #9739, .T. ) ;
#553 = VERTEX_POINT ( 'NONE', #5596 ) ;
#554 = DIRECTION ( 'NONE',  ( 0.000000000000000000, 0.000000000000000000, 1.000000000000000000 ) ) ;
#555 = ORIENTED_EDGE ( 'NONE', *, *, #7128, .T. ) ;
#556 = AXIS2_PLACEMENT_3D ( 'NONE', #2349, #4217, #11140 ) ;
#557 = DIRECTION ( 'NONE',  ( -1.000000000000000000, 0.000000000000000000, 0.000000000000000000 ) ) ;
#558 = VECTOR ( 'NONE', #12526, 1000.000000000000000 ) ;
#559 = EDGE_CURVE ( 'NONE', #12638, #14575, #4895, .T. ) ;
#560 = DIRECTION ( 'NONE',  ( 0.000000000000000000, 0.000000000000000000, -1.000000000000000000 ) ) ;
#561 = TOROIDAL_SURFACE ( 'NONE', #15532, 3.606799999999999784, 0.7620000000000000107 ) ;
#562 = ORIENTED_EDGE ( 'NONE', *, *, #9428, .T. ) ;
#563 = DIRECTION ( 'NONE',  ( 1.000000000000000000, 0.000000000000000000, 0.000000000000000000 ) ) ;
#564 = CARTESIAN_POINT ( 'NONE',  ( 9.855199999999999960, -3639.502500000000055, 2263.571799999999712 ) ) ;
#565 = VERTEX_POINT ( 'NONE', #2407 ) ;
#566 = CARTESIAN_POINT ( 'NONE',  ( 133.2229999999989900, -3579.494999999999891, 2239.771999999999935 ) ) ;
#567 = CARTESIAN_POINT ( 'NONE',  ( 11.34365660141000021, -3597.148244321000220, 2296.210799999999836 ) ) ;
#568 = ORIENTED_EDGE ( 'NONE', *, *, #1578, .T. ) ;
#569 = CARTESIAN_POINT ( 'NONE',  ( 127.0000000000000000, -3619.500000000000000, 2239.771999999999935 ) ) ;
#570 = PRODUCT_DEFINITION_CONTEXT ( 'detailed design', #18003, 'design' ) ;
#571 = AXIS2_PLACEMENT_3D ( 'NONE', #16730, #14869, #10564 ) ;
#572 = VERTEX_POINT ( 'NONE', #14610 ) ;
#573 = B_SPLINE_CURVE_WITH_KNOTS ( 'NONE', 3,
 ( #8571, #6467, #2818, #12194, #6355, #17224, #3164, #8457, #6587, #4928, #17460, #6814, #19231, #11959, #13955, #4695, #17114, #22735, #1290, #13608, #21105, #10199, #10317, #13841, #5050, #20988, #17338, #15366, #12074, #1412, #19346, #16993, #13728, #943, #11845, #10078, #8335, #8216, #4579, #15480, #22380 ),
 .UNSPECIFIED., .F., .F.,
 ( 4, 2, 2, 1, 1, 2, 2, 2, 2, 1, 1, 1, 2, 2, 2, 2, 2, 2, 2, 1, 1, 2, 2, 4 ),
 ( 0.000000000000000000, 0.1249999999964153119, 0.1874999999948339380, 0.2187499999938449513, 0.2343749999936358408, 0.2421874999938173900, 0.2499999999939989115, 0.3749999999956662444, 0.4374999999964459541, 0.4687499999966819875, 0.4843749999968000042, 0.4921874999968590125, 0.4960937499968964826, 0.4999999999969340081, 0.5624999999948754326, 0.5937499999937037032, 0.6249999999925319738, 0.6874999999899414904, 0.7187499999887656532, 0.7343749999881804547, 0.7421874999878907975, 0.7460937499877459134, 0.7499999999876010293, 1.000000000000000000 ),
 .UNSPECIFIED. ) ;
#574 = FACE_OUTER_BOUND ( 'NONE', #9837, .T. ) ;
#575 = AXIS2_PLACEMENT_3D ( 'NONE', #15230, #18852, #11820 ) ;
#576 = PERSON_AND_ORGANIZATION ( #5446, #1895 ) ;
#577 = EDGE_CURVE ( 'NONE', #10134, #2356, #17622, .T. ) ;
#578 = AXIS2_PLACEMENT_3D ( 'NONE', #5509, #9011, #16610 ) ;
#579 = AXIS2_PLACEMENT_3D ( 'NONE', #12558, #10797, #10682 ) ;
#580 = DIRECTION ( 'NONE',  ( 0.000000000000000000, 0.000000000000000000, 1.000000000000000000 ) ) ;
#581 = LINE ( 'NONE', #9484, #20792 ) ;
#582 = DIRECTION ( 'NONE',  ( 0.8660254037825247941, -0.5000000000033149039, -5.278136500991149341E-12 ) ) ;
#583 = CARTESIAN_POINT ( 'NONE',  ( 11.61864837389999927, -3576.858790609000152, 2257.644359388999874 ) ) ;
#584 = CARTESIAN_POINT ( 'NONE',  ( 142.2297613316639797, -3578.193174660338627, 2250.157761700695119 ) ) ;
#585 = EDGE_LOOP ( 'NONE', ( #11944, #15585, #11993, #17143 ) ) ;
#586 = B_SPLINE_CURVE_WITH_KNOTS ( 'NONE', 3,
 ( #14737, #5248, #12392, #19538, #3477, #12506 ),
 .UNSPECIFIED., .F., .F.,
 ( 4, 1, 1, 4 ),
 ( 0.000000000000000000, 0.3333333333333000081, 0.6666666666667000474, 1.000000000000000000 ),
 .UNSPECIFIED. ) ;
#587 = ORIENTED_EDGE ( 'NONE', *, *, #13824, .T. ) ;
#588 = CARTESIAN_POINT ( 'NONE',  ( 10.36831320290272984, -3598.151299999887669, 2296.210799999999836 ) ) ;
#589 = ORIENTED_EDGE ( 'NONE', *, *, #12880, .F. ) ;
#590 = CARTESIAN_POINT ( 'NONE',  ( 15.48106175502000070, -3598.871388315999866, 2279.464089773000069 ) ) ;
#591 = CARTESIAN_POINT ( 'NONE',  ( 142.5448000000000093, -3659.504999999999654, 2256.063560000000052 ) ) ;
#592 = APPLIED_PERSON_AND_ORGANIZATION_ASSIGNMENT ( #3598, #12283, ( #16852 ) ) ;
#593 = AXIS2_PLACEMENT_3D ( 'NONE', #5374, #17902, #21270 ) ;
#594 = ORIENTED_EDGE ( 'NONE', *, *, #22385, .F. ) ;
#595 = AXIS2_PLACEMENT_3D ( 'NONE', #12987, #7589, #14400 ) ;
#596 = ORIENTED_EDGE ( 'NONE', *, *, #22546, .F. ) ;
#597 = CARTESIAN_POINT ( 'NONE',  ( 57.14999999999999858, -3543.300000000000182, 2251.506800000000112 ) ) ;
#598 = EDGE_LOOP ( 'NONE', ( #2863, #2197, #6752, #20467 ) ) ;
#599 = DIRECTION ( 'NONE',  ( 0.000000000000000000, 0.000000000000000000, 1.000000000000000000 ) ) ;
#600 = CARTESIAN_POINT ( 'NONE',  ( 14.56785476897627341, -3577.348371727691301, 2249.802387783117410 ) ) ;
#601 = CARTESIAN_POINT ( 'NONE',  ( 141.5643557054172845, -3581.643940524072150, 2246.800655991665735 ) ) ;
#602 = ORIENTED_EDGE ( 'NONE', *, *, #20236, .T. ) ;
#603 = CARTESIAN_POINT ( 'NONE',  ( 12.69999999999999929, -3659.504999999999654, 2245.359999999999673 ) ) ;
#604 = PERSON_AND_ORGANIZATION ( #5446, #1895 ) ;
#605 = CARTESIAN_POINT ( 'NONE',  ( 20.43202061276000236, -3694.678775005999796, 2260.577432963000319 ) ) ;
#606 = DIRECTION ( 'NONE',  ( -2.324635735433000053E-14, 2.336881798971000105E-14, -1.000000000000000000 ) ) ;
#607 = DIRECTION ( 'NONE',  ( 0.000000000000000000, 1.000000000000000000, 0.000000000000000000 ) ) ;
#608 = AXIS2_PLACEMENT_3D ( 'NONE', #1214, #8376, #22656 ) ;
#609 = AXIS2_PLACEMENT_3D ( 'NONE', #5564, #4025, #11052 ) ;
#610 = DIRECTION ( 'NONE',  ( 0.000000000000000000, 0.000000000000000000, -1.000000000000000000 ) ) ;
#611 = AXIS2_PLACEMENT_3D ( 'NONE', #16670, #22278, #6258 ) ;
#612 = ORIENTED_EDGE ( 'NONE', *, *, #10651, .T. ) ;
#613 = CARTESIAN_POINT ( 'NONE',  ( 141.7318470609411065, -3661.497086795617179, 2249.892725811761011 ) ) ;
#614 = ORIENTED_EDGE ( 'NONE', *, *, #19767, .F. ) ;
#615 = AXIS2_PLACEMENT_3D ( 'NONE', #11553, #18701, #2651 ) ;
#616 = ORIENTED_EDGE ( 'NONE', *, *, #16446, .F. ) ;
#617 = ORIENTED_EDGE ( 'NONE', *, *, #76, .T. ) ;
#618 = PRODUCT_RELATED_PRODUCT_CATEGORY ( 'detail', '', ( #12377 ) ) ;
#619 = DIRECTION ( 'NONE',  ( -1.000000000000000000, 0.000000000000000000, 0.000000000000000000 ) ) ;
#620 = EDGE_CURVE ( 'NONE', #3298, #2966, #20610, .T. ) ;
#621 = ORIENTED_EDGE ( 'NONE', *, *, #8439, .F. ) ;
#622 = ORIENTED_EDGE ( 'NONE', *, *, #5424, .F. ) ;
#623 = CARTESIAN_POINT ( 'NONE',  ( 147.3199999999999932, -3544.570000000000164, 2260.600000000000364 ) ) ;
#624 = DIRECTION ( 'NONE',  ( 0.000000000000000000, 0.000000000000000000, -1.000000000000000000 ) ) ;
#625 = ORIENTED_EDGE ( 'NONE', *, *, #3214, .F. ) ;
#626 = AXIS2_PLACEMENT_3D ( 'NONE', #6837, #15624, #3186 ) ;
#627 = DIRECTION ( 'NONE',  ( 0.000000000000000000, 0.000000000000000000, 1.000000000000000000 ) ) ;
#628 = EDGE_CURVE ( 'NONE', #15285, #22614, #15174, .T. ) ;
#629 = DIRECTION ( 'NONE',  ( -1.000000000000000000, 0.000000000000000000, 0.000000000000000000 ) ) ;
#630 = CARTESIAN_POINT ( 'NONE',  ( 145.3796772601000100, -3660.139769217999856, 2244.548186305999934 ) ) ;
#631 = EDGE_CURVE ( 'NONE', #20297, #452, #17568, .T. ) ;
#632 = DIRECTION ( 'NONE',  ( 1.000000000000000000, 0.000000000000000000, 0.000000000000000000 ) ) ;
#633 = PERSON_AND_ORGANIZATION_ROLE ( 'design_owner' ) ;
#634 = EDGE_CURVE ( 'NONE', #10444, #22942, #12024, .T. ) ;
#635 = AXIS2_PLACEMENT_3D ( 'NONE', #7672, #12951, #21744 ) ;
#636 = DIRECTION ( 'NONE',  ( 0.000000000000000000, -1.000000000000000000, 0.000000000000000000 ) ) ;
#637 = DIRECTION ( 'NONE',  ( -1.000000000000000000, 0.000000000000000000, 0.000000000000000000 ) ) ;
#638 = DIRECTION ( 'NONE',  ( -1.000000000000000000, 0.000000000000000000, 0.000000000000000000 ) ) ;
#639 = ADVANCED_FACE ( 'NONE', ( #13525 ), #4161, .T. ) ;
#640 = ORIENTED_EDGE ( 'NONE', *, *, #11917, .T. ) ;
#641 = AXIS2_PLACEMENT_3D ( 'NONE', #16401, #9374, #7492 ) ;
#642 = DIRECTION ( 'NONE',  ( 0.000000000000000000, 0.000000000000000000, -1.000000000000000000 ) ) ;
#643 = TOROIDAL_SURFACE ( 'NONE', #13371, 5.080000000000000071, 0.3810000000000000053 ) ;
#644 = DIRECTION ( 'NONE',  ( 0.8660254037825932949, 0.5000000000031962211, 0.000000000000000000 ) ) ;
#645 = ORIENTED_EDGE ( 'NONE', *, *, #5737, .F. ) ;
#646 = PLANE ( 'NONE',  #2051 ) ;
#647 = ORIENTED_EDGE ( 'NONE', *, *, #17355, .T. ) ;
#648 = CARTESIAN_POINT ( 'NONE',  ( 18.35682388039437640, -3658.691851779573881, 2244.943199301839741 ) ) ;
#649 = AXIS2_PLACEMENT_3D ( 'NONE', #3890, #6955, #18185 ) ;
#650 = VERTEX_POINT ( 'NONE', #22192 ) ;
#651 = ORIENTED_EDGE ( 'NONE', *, *, #14900, .F. ) ;
#652 = DIRECTION ( 'NONE',  ( -1.000000000000000000, 0.000000000000000000, 0.000000000000000000 ) ) ;
#653 = AXIS2_PLACEMENT_3D ( 'NONE', #7513, #14669, #21470 ) ;
#654 = DIRECTION ( 'NONE',  ( 0.000000000000000000, -1.000000000000000000, 0.000000000000000000 ) ) ;
#655 = CARTESIAN_POINT ( 'NONE',  ( 111.4552000000009997, -3644.899999999999636, 2261.869999999999891 ) ) ;
#656 = DIRECTION ( 'NONE',  ( -1.000000000000000000, 0.000000000000000000, 0.000000000000000000 ) ) ;
#657 = CARTESIAN_POINT ( 'NONE',  ( 10.36831320284000135, -3638.156300000000101, 2292.781800000000203 ) ) ;
#658 = CARTESIAN_POINT ( 'NONE',  ( 20.37014473194848918, -3695.033231289878131, 2260.474410595720656 ) ) ;
#659 = ORIENTED_EDGE ( 'NONE', *, *, #20177, .T. ) ;
#660 = PERSON_AND_ORGANIZATION ( #5446, #1895 ) ;
#661 = ADVANCED_FACE ( 'NONE', ( #9884 ), #22307, .T. ) ;
#662 = CIRCLE ( 'NONE', #16384, 11.11250000000000071 ) ;
#663 = ORIENTED_EDGE ( 'NONE', *, *, #15516, .F. ) ;
#664 = CARTESIAN_POINT ( 'NONE',  ( 145.1453925538234273, -3657.768934968029953, 2245.814674103072775 ) ) ;
#665 = AXIS2_PLACEMENT_3D ( 'NONE', #11297, #7552, #21854 ) ;
#666 = CARTESIAN_POINT ( 'NONE',  ( 9.913021306595382498, -3580.067331691507206, 2249.967926883056407 ) ) ;
#667 = LINE ( 'NONE', #14627, #2267 ) ;
#668 = ORIENTED_EDGE ( 'NONE', *, *, #15029, .F. ) ;
#669 = CARTESIAN_POINT ( 'NONE',  ( 134.0204252830999962, -3660.140268639000169, 2244.547525601999951 ) ) ;
#670 = CARTESIAN_POINT ( 'NONE',  ( 9.652920519510999497, -3695.699999999999818, 2254.503999999999905 ) ) ;
#671 = VERTEX_POINT ( 'NONE', #9668 ) ;
#672 =( BOUNDED_CURVE ( )  B_SPLINE_CURVE ( 3, ( #2113, #7152, #5395, #8907 ),
 .UNSPECIFIED., .F., .T. ) 
 B_SPLINE_CURVE_WITH_KNOTS ( ( 4, 4 ),
 ( 1.570796326475431659, 3.141592653589783346 ),
 .UNSPECIFIED. ) 
 CURVE ( )  GEOMETRIC_REPRESENTATION_ITEM ( )  RATIONAL_B_SPLINE_CURVE ( ( 1.000000000000000000, 0.8047378540490687238, 0.8047378540490687238, 1.000000000000000000 ) ) 
 REPRESENTATION_ITEM ( '' )  );
#673 = DIRECTION ( 'NONE',  ( -0.000000000000000000, 1.000000000000000000, 0.000000000000000000 ) ) ;
#674 = CARTESIAN_POINT ( 'NONE',  ( 13.60653736635324762, -3662.201562304035178, 2249.352418353455505 ) ) ;
#675 = CIRCLE ( 'NONE', #12272, 3.606800000000000228 ) ;
#676 = LINE ( 'NONE', #22333, #5098 ) ;
#677 = ORIENTED_EDGE ( 'NONE', *, *, #19546, .F. ) ;
#678 = DIRECTION ( 'NONE',  ( 0.000000000000000000, 0.000000000000000000, -1.000000000000000000 ) ) ;
#679 = DIRECTION ( 'NONE',  ( 1.000000000000000000, 0.000000000000000000, 0.000000000000000000 ) ) ;
#680 = ORIENTED_EDGE ( 'NONE', *, *, #11726, .T. ) ;
#681 = DIRECTION ( 'NONE',  ( -1.000000000000000000, 0.000000000000000000, 0.000000000000000000 ) ) ;
#682 = CYLINDRICAL_SURFACE ( 'NONE', #10572, 2.844800000000001550 ) ;
#683 = B_SPLINE_CURVE_WITH_KNOTS ( 'NONE', 3,
 ( #20967, #4674, #15583, #4912, #10968, #9219, #12727, #19881, #9444, #11089, #193, #4051, #12620, #11197, #19772, #16699, #4164, #425, #21750, #7344, #13070, #14726, #20221, #21863, #12959, #2187, #7564, #16360, #5708, #20001, #1949 ),
 .UNSPECIFIED., .F., .F.,
 ( 4, 2, 2, 2, 2, 2, 1, 2, 2, 2, 2, 1, 1, 2, 2, 2, 4 ),
 ( 0.000000000000000000, 0.1249999999996052324, 0.1874999999994706734, 0.2499999999993361421, 0.3749999999984279242, 0.4374999999981442622, 0.4687499999978084197, 0.4843749999976455500, 0.4999999999974826803, 0.6249999999991210364, 0.6874999999997667421, 0.7187499999998425704, 0.7343750000001272316, 0.7421875000001436629, 0.7500000000001599831, 0.8750000000000800471, 1.000000000000000000 ),
 .UNSPECIFIED. ) ;
#684 = EDGE_LOOP ( 'NONE', ( #19969, #16210, #13476, #14572, #12675, #15722, #4180, #12665 ) ) ;
#685 = ORIENTED_EDGE ( 'NONE', *, *, #9708, .F. ) ;
#686 = CARTESIAN_POINT ( 'NONE',  ( 20.82707948048999924, -3695.699999999999818, 2259.329999999999927 ) ) ;
#687 = ORIENTED_EDGE ( 'NONE', *, *, #12448, .F. ) ;
#688 = CARTESIAN_POINT ( 'NONE',  ( 145.3843004971977564, -3580.087277415173048, 2244.825193658660282 ) ) ;
#689 = CALENDAR_DATE ( 2026, 26, 10 ) ;
#690 = EDGE_CURVE ( 'NONE', #10874, #18714, #15406, .T. ) ;
#691 = EDGE_CURVE ( 'NONE', #20500, #3687, #20338, .T. ) ;
#692 = DIRECTION ( 'NONE',  ( -1.000000000000000000, 0.000000000000000000, 0.000000000000000000 ) ) ;
#693 = EDGE_CURVE ( 'NONE', #7794, #10683, #1154, .T. ) ;
#694 = CARTESIAN_POINT ( 'NONE',  ( 17.56334821106831967, -3662.506481300412815, 2245.813177206671298 ) ) ;
#695 = DIRECTION ( 'NONE',  ( -2.848935406719999894E-12, 1.000000000000000000, 2.336881798978000141E-14 ) ) ;
#696 = LINE ( 'NONE', #18724, #15131 ) ;
#697 = ADVANCED_FACE ( 'NONE', ( #2864 ), #13179, .T. ) ;
#698 = VERTEX_POINT ( 'NONE', #22418 ) ;
#699 = LINE ( 'NONE', #4216, #9234 ) ;
#700 = ORIENTED_EDGE ( 'NONE', *, *, #6839, .T. ) ;
#701 = ORIENTED_EDGE ( 'NONE', *, *, #13282, .T. ) ;
#702 = CARTESIAN_POINT ( 'NONE',  ( 14.71622495092000094, -3597.481870621000326, 2279.634028774999933 ) ) ;
#703 = PERSON ( 'NAUO-PER12', 'UNSPECIFIED', 'UNSPECIFIED', ('UNSPECIFIED'), ('UNSPECIFIED'), ('UNSPECIFIED') ) ;
#704 = CARTESIAN_POINT ( 'NONE',  ( 15.70174596896855057, -3543.300000000022010, 2254.617539517661498 ) ) ;
#705 = EDGE_CURVE ( 'NONE', #12409, #21968, #18378, .T. ) ;
#706 = EDGE_CURVE ( 'NONE', #19558, #12468, #18680, .T. ) ;
#707 = ORIENTED_EDGE ( 'NONE', *, *, #22875, .T. ) ;
#708 = AXIS2_PLACEMENT_3D ( 'NONE', #9587, #453, #16733 ) ;
#709 = ORIENTED_EDGE ( 'NONE', *, *, #3573, .F. ) ;
#710 = LINE ( 'NONE', #15013, #21202 ) ;
#711 = CARTESIAN_POINT ( 'NONE',  ( 11.57570654715081737, -3576.881424651616726, 2249.436186243917291 ) ) ;
#712 = CARTESIAN_POINT ( 'NONE',  ( 0.000000000000000000, 0.000000000000000000, 0.000000000000000000 ) ) ;
#713 = CARTESIAN_POINT ( 'NONE',  ( 141.7107714205274931, -3581.507805183896835, 2248.433351161166229 ) ) ;
#714 = ORIENTED_EDGE ( 'NONE', *, *, #9491, .T. ) ;
#715 = CARTESIAN_POINT ( 'NONE',  ( -12.31900000000001505, -3577.513799999857383, 2249.723686796824950 ) ) ;
#716 = APPROVAL_DATE_TIME ( #2368, #6342 ) ;
#717 = LINE ( 'NONE', #21821, #6652 ) ;
#718 = CARTESIAN_POINT ( 'NONE',  ( 0.000000000000000000, -3694.938000000000102, 2238.248000000000047 ) ) ;
#719 = CARTESIAN_POINT ( 'NONE',  ( 136.8551930557000276, -3659.332964842520141, 2250.125630000906767 ) ) ;
#720 = ORIENTED_EDGE ( 'NONE', *, *, #5225, .T. ) ;
#721 = AXIS2_PLACEMENT_3D ( 'NONE', #17891, #3471, #10623 ) ;
#722 = ORIENTED_EDGE ( 'NONE', *, *, #10015, .F. ) ;
#723 = FACE_OUTER_BOUND ( 'NONE', #15167, .T. ) ;
#724 = VERTEX_POINT ( 'NONE', #18794 ) ;
#725 = LINE ( 'NONE', #14924, #438 ) ;
#726 = CARTESIAN_POINT ( 'NONE',  ( 133.2229999999999848, -3659.504999999999654, 2239.771999999999935 ) ) ;
#727 = ORIENTED_EDGE ( 'NONE', *, *, #369, .T. ) ;
#728 = CARTESIAN_POINT ( 'NONE',  ( 7.003448455909224712, -3659.044352728992635, 2244.765892648666977 ) ) ;
#729 = DIRECTION ( 'NONE',  ( 0.000000000000000000, -1.000000000000000000, 0.000000000000000000 ) ) ;
#730 = LOCAL_TIME ( 17, 37, 43.00000000000000000, #20623 ) ;
#731 = CIRCLE ( 'NONE', #1095, 4.114799999999974034 ) ;
#732 = CARTESIAN_POINT ( 'NONE',  ( 18.16100000000000136, -3579.494999999999891, 2244.978999999999814 ) ) ;
#733 = PERSON_AND_ORGANIZATION ( #5446, #1895 ) ;
#734 = CARTESIAN_POINT ( 'NONE',  ( 12.69999999999999929, -3579.494999999999891, 2246.630000000000109 ) ) ;
#735 = APPLIED_PERSON_AND_ORGANIZATION_ASSIGNMENT ( #7605, #2453, ( #16881 ) ) ;
#736 = CARTESIAN_POINT ( 'NONE',  ( 142.4974789541179234, -3658.986641539371703, 2249.992541019687451 ) ) ;
#737 = DIRECTION ( 'NONE',  ( 0.000000000000000000, -1.000000000000000000, 0.000000000000000000 ) ) ;
#738 = ORIENTED_EDGE ( 'NONE', *, *, #22032, .F. ) ;
#739 = CARTESIAN_POINT ( 'NONE',  ( 3.048000000000000043, -3694.938000000000102, 2239.009999999999764 ) ) ;
#740 = EDGE_CURVE ( 'NONE', #9155, #17917, #6159, .T. ) ;
#741 = PRODUCT_DEFINITION_FORMATION_WITH_SPECIFIED_SOURCE ( 'ANY', '', #20975, .NOT_KNOWN. ) ;
#742 = EDGE_CURVE ( 'NONE', #4653, #946, #14644, .T. ) ;
#743 = DIRECTION ( 'NONE',  ( 0.000000000000000000, 0.000000000000000000, 1.000000000000000000 ) ) ;
#744 = ORIENTED_EDGE ( 'NONE', *, *, #18244, .F. ) ;
#745 = DIRECTION ( 'NONE',  ( 0.000000000000000000, 0.000000000000000000, 1.000000000000000000 ) ) ;
#746 = EDGE_CURVE ( 'NONE', #18142, #1451, #22119, .T. ) ;
#747 = CARTESIAN_POINT ( 'NONE',  ( 18.33711823532055973, -3658.564445501008322, 2245.022483595459107 ) ) ;
#748 = ORIENTED_EDGE ( 'NONE', *, *, #10145, .F. ) ;
#749 = VERTEX_POINT ( 'NONE', #20786 ) ;
#750 = TOROIDAL_SURFACE ( 'NONE', #3747, 3.606799999999999784, 0.7620000000000000107 ) ;
#751 = DIRECTION ( 'NONE',  ( 0.000000000000000000, -0.8660254037817188832, 0.5000000000047110094 ) ) ;
#752 = CARTESIAN_POINT ( 'NONE',  ( 117.1447999999989946, -3644.899999999999636, 2239.771999999999935 ) ) ;
#753 = DIRECTION ( 'NONE',  ( -0.7071067811865975328, 0.000000000000000000, 0.7071067811864976127 ) ) ;
#754 = CARTESIAN_POINT ( 'NONE',  ( 127.0000000000000000, -3660.140000000000327, 2244.547199999999975 ) ) ;
#755 = DIRECTION ( 'NONE',  ( 0.000000000000000000, 0.000000000000000000, 1.000000000000000000 ) ) ;
#756 = CARTESIAN_POINT ( 'NONE',  ( 101.5999999999999943, -3670.300000000000182, 2239.771999999999935 ) ) ;
#757 = CARTESIAN_POINT ( 'NONE',  ( 20.82707948048999924, -3695.699999999999818, 2259.329999999999927 ) ) ;
#758 = EDGE_LOOP ( 'NONE', ( #7533, #4820 ) ) ;
#760 = AXIS2_PLACEMENT_3D ( 'NONE', #9119, #16259, #5610 ) ;
#759 = COORDINATED_UNIVERSAL_TIME_OFFSET ( 0, 0, .AHEAD. ) ;
#761 = DIRECTION ( 'NONE',  ( 1.224646799141920914E-16, -1.000000000000000000, -2.336881798971000421E-14 ) ) ;
#762 = EDGE_CURVE ( 'NONE', #1396, #13309, #12722, .T. ) ;
#763 = APPROVAL_PERSON_ORGANIZATION ( #1285, #16363, #17218 ) ;
#764 = CARTESIAN_POINT ( 'NONE',  ( 1.270000000000000018, -3660.140000000000327, 2250.236800000000130 ) ) ;
#765 = AXIS2_PLACEMENT_3D ( 'NONE', #17214, #2932, #21303 ) ;
#766 = CARTESIAN_POINT ( 'NONE',  ( 0.000000000000000000, -3543.299999999999727, 2254.250000000000000 ) ) ;
#767 = VERTEX_POINT ( 'NONE', #4738 ) ;
#768 = LINE ( 'NONE', #7930, #7396 ) ;
#769 = ADVANCED_FACE ( 'NONE', ( #9773 ), #6049, .T. ) ;
#770 = CARTESIAN_POINT ( 'NONE',  ( 3.810000000000000053, -3694.938000000000102, 2238.248000000000047 ) ) ;
#771 = CARTESIAN_POINT ( 'NONE',  ( 134.9056831650161712, -3576.384005279409848, 2245.990590281915502 ) ) ;
#772 = EDGE_LOOP ( 'NONE', ( #1178, #16136, #20200, #22962 ) ) ;
#773 = DIRECTION ( 'NONE',  ( 0.000000000000000000, 0.000000000000000000, -1.000000000000000000 ) ) ;
#774 = EDGE_CURVE ( 'NONE', #11858, #19931, #1566, .T. ) ;
#775 = CARTESIAN_POINT ( 'NONE',  ( 14.60105122252583598, -3661.621915575120056, 2249.820482541457750 ) ) ;
#776 = EDGE_CURVE ( 'NONE', #11037, #16275, #8276, .T. ) ;
#777 = DIRECTION ( 'NONE',  ( 0.000000000000000000, 1.000000000000000000, 0.000000000000000000 ) ) ;
#778 = ORIENTED_EDGE ( 'NONE', *, *, #12253, .T. ) ;
#779 = ORGANIZATION ( 'NAUO-ORG10', 'UNSPECIFIED', 'UNSPECIFIED' ) ;
#780 = DIRECTION ( 'NONE',  ( 0.000000000000000000, 0.000000000000000000, 1.000000000000000000 ) ) ;
#781 = FACE_BOUND ( 'NONE', #2465, .T. ) ;
#782 = CARTESIAN_POINT ( 'NONE',  ( 15.03168679706394428, -3598.151299999898129, 2296.210799999999836 ) ) ;
#783 = DIRECTION ( 'NONE',  ( 0.000000000000000000, 0.000000000000000000, -1.000000000000000000 ) ) ;
#784 = EDGE_LOOP ( 'NONE', ( #6046, #14713, #447, #10205, #13619, #10680, #15703, #15282 ) ) ;
#785 = PRODUCT ( 'Hinge 1', 'Hinge 1', '', ( #12191 ) ) ;
#786 = VECTOR ( 'NONE', #17705, 1000.000000000000000 ) ;
#787 = DIRECTION ( 'NONE',  ( 0.000000000000000000, 0.000000000000000000, 1.000000000000000000 ) ) ;
#788 = ORIENTED_EDGE ( 'NONE', *, *, #18877, .T. ) ;
#789 = CARTESIAN_POINT ( 'NONE',  ( 22.54063073453000143, -3543.299999999999727, 2275.763800000000174 ) ) ;
#790 = COORDINATED_UNIVERSAL_TIME_OFFSET ( 0, 0, .AHEAD. ) ;
#791 = CARTESIAN_POINT ( 'NONE',  ( 145.4031900104867532, -3579.124489882064609, 2244.559018039585226 ) ) ;
#792 = CARTESIAN_POINT ( 'NONE',  ( 18.21505860824958489, -3661.003409629256566, 2244.681372502921931 ) ) ;
#793 = FACE_OUTER_BOUND ( 'NONE', #14812, .T. ) ;
#794 = DIRECTION ( 'NONE',  ( 0.000000000000000000, 0.000000000000000000, 1.000000000000000000 ) ) ;
#795 = CARTESIAN_POINT ( 'NONE',  ( 137.3409534416252882, -3577.904103566719641, 2250.071838006614144 ) ) ;
#796 = VERTEX_POINT ( 'NONE', #19151 ) ;
#797 = CIRCLE ( 'NONE', #11314, 2.844799999999994444 ) ;
#798 = DIRECTION ( 'NONE',  ( -5.682243826821398966E-14, -1.000000000000000000, 0.000000000000000000 ) ) ;
#799 = EDGE_CURVE ( 'NONE', #13105, #20246, #7087, .T. ) ;
#800 = AXIS2_PLACEMENT_3D ( 'NONE', #22482, #19562, #14530 ) ;
#801 = CARTESIAN_POINT ( 'NONE',  ( 35.25520000000000209, -3644.899999999999636, 2261.869999999999891 ) ) ;
#802 = ORIENTED_EDGE ( 'NONE', *, *, #4244, .F. ) ;
#803 = CARTESIAN_POINT ( 'NONE',  ( 41.70680000000000121, -3594.099999999999909, 2259.837999999999738 ) ) ;
#804 = CARTESIAN_POINT ( 'NONE',  ( 15.56736770577728812, -3543.382189095376816, 2254.953892137616549 ) ) ;
#805 = ADVANCED_FACE ( 'NONE', ( #15870 ), #10238, .T. ) ;
#806 = ORIENTED_EDGE ( 'NONE', *, *, #17445, .T. ) ;
#807 = ADVANCED_FACE ( 'NONE', ( #6629 ), #3773, .T. ) ;
#808 = ORIENTED_EDGE ( 'NONE', *, *, #6925, .T. ) ;
#809 = ORIENTED_EDGE ( 'NONE', *, *, #15098, .F. ) ;
#810 = CARTESIAN_POINT ( 'NONE',  ( 12.69999999999999929, -3589.528000000000247, 2268.705139999999574 ) ) ;
#811 = AXIS2_PLACEMENT_3D ( 'NONE', #210, #439, #20016 ) ;
#812 = EDGE_LOOP ( 'NONE', ( #1054, #19308, #16094, #2835 ) ) ;
#813 = CARTESIAN_POINT ( 'NONE',  ( 10.16000000000000014, -3544.570000000000164, 2255.774000000000342 ) ) ;
#814 = CARTESIAN_POINT ( 'NONE',  ( 13.24259552251218253, -3576.687580108851762, 2249.232770475404322 ) ) ;
#815 = DIRECTION ( 'NONE',  ( 1.000000000000000000, 0.000000000000000000, 0.000000000000000000 ) ) ;
#816 = CARTESIAN_POINT ( 'NONE',  ( 141.4866483936817474, -3581.708819005992609, 2247.454754559452795 ) ) ;
#817 = TOROIDAL_SURFACE ( 'NONE', #3822, 1.905000000000000027, 1.270000000000000018 ) ;
#818 = EDGE_CURVE ( 'NONE', #8027, #749, #22847, .T. ) ;
#819 = VERTEX_POINT ( 'NONE', #8838 ) ;
#821 = DIRECTION ( 'NONE',  ( 0.000000000000000000, 0.000000000000000000, 1.000000000000000000 ) ) ;
#820 = AXIS2_PLACEMENT_3D ( 'NONE', #17542, #22924, #10165 ) ;
#822 = PERSON_AND_ORGANIZATION_ROLE ( 'creator' ) ;
#823 = AXIS2_PLACEMENT_3D ( 'NONE', #8783, #454, #20150 ) ;
#824 = CARTESIAN_POINT ( 'NONE',  ( 12.69999245750678263, -3602.342301254329868, 2279.817638608992183 ) ) ;
#825 = VERTEX_POINT ( 'NONE', #10356 ) ;
#826 = CARTESIAN_POINT ( 'NONE',  ( 20.66695186275289586, -3543.364998063555959, 2259.731097527611382 ) ) ;
#827 = EDGE_CURVE ( 'NONE', #13681, #7121, #20278, .T. ) ;
#828 = CARTESIAN_POINT ( 'NONE',  ( 137.4277150837954196, -3577.744018727676121, 2257.824198891456490 ) ) ;
#829 = EDGE_CURVE ( 'NONE', #8062, #928, #9069, .T. ) ;
#830 = VERTEX_POINT ( 'NONE', #15641 ) ;
#831 = AXIS2_PLACEMENT_3D ( 'NONE', #4811, #14196, #10553 ) ;
#832 = DIRECTION ( 'NONE',  ( 0.000000000000000000, 0.000000000000000000, 1.000000000000000000 ) ) ;
#833 = VERTEX_POINT ( 'NONE', #22769 ) ;
#834 = ORIENTED_EDGE ( 'NONE', *, *, #2199, .T. ) ;
#835 = AXIS2_PLACEMENT_3D ( 'NONE', #10017, #9888, #2633 ) ;
#836 = AXIS2_PLACEMENT_3D ( 'NONE', #12560, #7289, #21924 ) ;
#837 = EDGE_CURVE ( 'NONE', #159, #10812, #12396, .T. ) ;
#838 = DIRECTION ( 'NONE',  ( -1.000000000000000000, 0.000000000000000000, 0.000000000000000000 ) ) ;
#839 = ORIENTED_EDGE ( 'NONE', *, *, #631, .T. ) ;
#840 = DIRECTION ( 'NONE',  ( 0.000000000000000000, -1.000000000000000000, 0.000000000000000000 ) ) ;
#841 = FACE_OUTER_BOUND ( 'NONE', #17125, .T. ) ;
#842 = ORIENTED_EDGE ( 'NONE', *, *, #14098, .T. ) ;
#843 = CARTESIAN_POINT ( 'NONE',  ( 7.127793039152298782, -3658.235454836550616, 2245.278666177176092 ) ) ;
#844 = CARTESIAN_POINT ( 'NONE',  ( 50.79999999999999716, -3619.500000000000000, 2260.600000000000364 ) ) ;
#845 = DIRECTION ( 'NONE',  ( 0.8660254037821217832, -0.5000000000040129011, 0.000000000000000000 ) ) ;
#846 = AXIS2_PLACEMENT_3D ( 'NONE', #22613, #20873, #1170 ) ;
#847 = CALENDAR_DATE ( 2026, 26, 10 ) ;
#848 = DIRECTION ( 'NONE',  ( 0.000000000000000000, 1.000000000000000000, 0.000000000000000000 ) ) ;
#849 = DIRECTION ( 'NONE',  ( -1.000000000000000000, 2.318894227180000040E-14, 2.343004830739999973E-14 ) ) ;
#850 = TOROIDAL_SURFACE ( 'NONE', #13965, 3.606799999999999784, 0.7620000000000000107 ) ;
#851 = ADVANCED_FACE ( 'NONE', ( #4969 ), #12116, .T. ) ;
#852 = AXIS2_PLACEMENT_3D ( 'NONE', #21590, #20065, #5891 ) ;
#853 = DIRECTION ( 'NONE',  ( 1.000000000000000000, -3.122111992759158343E-13, 0.000000000000000000 ) ) ;
#854 = EDGE_LOOP ( 'NONE', ( #8023, #7975, #7190, #21142 ) ) ;
#855 = CARTESIAN_POINT ( 'NONE',  ( 137.1478751023463474, -3544.290797603923693, 2255.743570596557220 ) ) ;
#856 = ORIENTED_EDGE ( 'NONE', *, *, #6594, .T. ) ;
#857 = AXIS2_PLACEMENT_3D ( 'NONE', #11933, #20845, #22816 ) ;
#858 = CARTESIAN_POINT ( 'NONE',  ( 140.0740604329243979, -3582.321215597040464, 2257.597438756844895 ) ) ;
#859 = DIRECTION ( 'NONE',  ( -1.000000000000000000, 0.000000000000000000, 0.000000000000000000 ) ) ;
#860 = ORIENTED_EDGE ( 'NONE', *, *, #20397, .T. ) ;
#861 = VERTEX_POINT ( 'NONE', #7315 ) ;
#862 = DIRECTION ( 'NONE',  ( 0.7249994335945011414, 0.000000000000000000, -0.6887494619146010688 ) ) ;
#863 = DIRECTION ( 'NONE',  ( 2.216404975961944229E-13, 0.5000000000040877302, 0.8660254037820787065 ) ) ;
#864 = AXIS2_PLACEMENT_3D ( 'NONE', #15935, #8563, #21219 ) ;
#865 = CARTESIAN_POINT ( 'NONE',  ( 9.919062418924999847, -3600.124156707000111, 2279.464122714000041 ) ) ;
#866 = APPLIED_DATE_AND_TIME_ASSIGNMENT ( #23153, #14390, ( #12016 ) ) ;
#867 = CLOSED_SHELL ( 'NONE', ( #14940, #12863, #19811, #19888, #18956, #9075, #9658, #16602, #7572, #8719, #20455, #11654, #2285, #18371, #8932, #20976, #21272, #17443, #7122, #8280, #17572, #9311, #22381, #422, #10868, #20015 ) ) ;
#868 = CARTESIAN_POINT ( 'NONE',  ( 0.7620000000000000107, -3695.699999999999818, 2238.248000000000047 ) ) ;
#869 = DIRECTION ( 'NONE',  ( 0.000000000000000000, 0.000000000000000000, -1.000000000000000000 ) ) ;
#870 = DIRECTION ( 'NONE',  ( 0.000000000000000000, -1.000000000000000000, 0.000000000000000000 ) ) ;
#871 = ORIENTED_EDGE ( 'NONE', *, *, #559, .F. ) ;
#872 = PERSON_AND_ORGANIZATION_ROLE ( 'creator' ) ;
#873 = CARTESIAN_POINT ( 'NONE',  ( 145.0770480762069781, -3657.568064249584950, 2246.174318179428155 ) ) ;
#874 = AXIS2_PLACEMENT_3D ( 'NONE', #21453, #5403, #3402 ) ;
#875 = CYLINDRICAL_SURFACE ( 'NONE', #3817, 2.844800000000091700 ) ;
#876 = CARTESIAN_POINT ( 'NONE',  ( 9.855099624826999971, -3659.717132568602665, 2250.213600093685272 ) ) ;
#877 = EDGE_LOOP ( 'NONE', ( #14414, #4341, #3151, #7613 ) ) ;
#878 = DIRECTION ( 'NONE',  ( 0.000000000000000000, -1.000000000000000000, 0.000000000000000000 ) ) ;
#879 = CARTESIAN_POINT ( 'NONE',  ( 151.1299999999999955, -3544.570000000000164, 2259.329999999999927 ) ) ;
#880 = DIRECTION ( 'NONE',  ( 1.000000000000000000, -0.000000000000000000, 1.224646799147353207E-16 ) ) ;
#881 = ORIENTED_EDGE ( 'NONE', *, *, #371, .F. ) ;
#882 = CARTESIAN_POINT ( 'NONE',  ( 85.29320000000001301, -3594.099999999999909, 2260.600000000000364 ) ) ;
#883 = CARTESIAN_POINT ( 'NONE',  ( 14.89040167505680401, -3661.320454366029480, 2249.980433560093843 ) ) ;
#884 = LINE ( 'NONE', #18944, #10321 ) ;
#885 = ORIENTED_EDGE ( 'NONE', *, *, #19026, .T. ) ;
#886 = LINE ( 'NONE', #16728, #13299 ) ;
#887 = AXIS2_PLACEMENT_3D ( 'NONE', #10637, #19084, #12172 ) ;
#888 = DIRECTION ( 'NONE',  ( 0.000000000000000000, 0.000000000000000000, -1.000000000000000000 ) ) ;
#889 = APPROVAL ( #19450, 'UNSPECIFIED' ) ;
#890 = DIRECTION ( 'NONE',  ( 0.000000000000000000, -1.000000000000000000, 0.000000000000000000 ) ) ;
#891 = AXIS2_PLACEMENT_3D ( 'NONE', #11198, #9334, #9445 ) ;
#892 = CARTESIAN_POINT ( 'NONE',  ( 10.28147353980999945, -3597.988101833999735, 2279.551731614000346 ) ) ;
#893 = DIRECTION ( 'NONE',  ( 0.000000000000000000, 0.000000000000000000, -1.000000000000000000 ) ) ;
#894 = VERTEX_POINT ( 'NONE', #19852 ) ;
#895 = EDGE_LOOP ( 'NONE', ( #856, #7799, #9527, #3867 ) ) ;
#896 = EDGE_CURVE ( 'NONE', #1677, #13988, #5664, .T. ) ;
#897 = CARTESIAN_POINT ( 'NONE',  ( 137.3683132029016178, -3580.841200000194931, 2239.167815367238745 ) ) ;
#898 = EDGE_CURVE ( 'NONE', #22077, #9946, #21383, .T. ) ;
#899 = ORIENTED_EDGE ( 'NONE', *, *, #15246, .T. ) ;
#900 = CARTESIAN_POINT ( 'NONE',  ( 145.1993249291396069, -3581.050454772452667, 2245.576347930728843 ) ) ;
#901 = DATE_AND_TIME ( #11807, #3742 ) ;
#902 = EDGE_CURVE ( 'NONE', #6944, #20781, #3036, .T. ) ;
#903 = CARTESIAN_POINT ( 'NONE',  ( 141.8426865414658664, -3577.614611570635589, 2257.800363196316084 ) ) ;
#904 = CARTESIAN_POINT ( 'NONE',  ( 12.69999999999999929, -3596.322499999999764, 2264.841800000000148 ) ) ;
#905 = CIRCLE ( 'NONE', #11387, 1.269999999999993356 ) ;
#906 = DIRECTION ( 'NONE',  ( 1.000000000000000000, 0.000000000000000000, 0.000000000000000000 ) ) ;
#907 = CIRCLE ( 'NONE', #20759, 3.175000000000149925 ) ;
#908 = DIRECTION ( 'NONE',  ( 0.000000000000000000, 0.000000000000000000, -1.000000000000000000 ) ) ;
#909 = VECTOR ( 'NONE', #12471, 1000.000000000000000 ) ;
#910 = EDGE_CURVE ( 'NONE', #22386, #17848, #19970, .T. ) ;
#911 = PLANE ( 'NONE',  #6522 ) ;
#912 = B_SPLINE_CURVE_WITH_KNOTS ( 'NONE', 3,
 ( #15628, #20771, #22755, #13981 ),
 .UNSPECIFIED., .F., .F.,
 ( 4, 4 ),
 ( 0.000000000000000000, 1.000000000000000000 ),
 .UNSPECIFIED. ) ;
#913 = ADVANCED_FACE ( 'NONE', ( #5567 ), #3673, .T. ) ;
#914 = ORIENTED_EDGE ( 'NONE', *, *, #14134, .T. ) ;
#915 = DIRECTION ( 'NONE',  ( 1.000000000000000000, 0.000000000000000000, 0.000000000000000000 ) ) ;
#916 = DIRECTION ( 'NONE',  ( 0.000000000000000000, 0.000000000000000000, -1.000000000000000000 ) ) ;
#917 = EDGE_LOOP ( 'NONE', ( #19607, #7311 ) ) ;
#918 = EDGE_CURVE ( 'NONE', #2972, #13491, #12004, .T. ) ;
#919 = CARTESIAN_POINT ( 'NONE',  ( 18.41519309055000164, -3659.504912144000173, 2244.618989493999834 ) ) ;
#920 = CARTESIAN_POINT ( 'NONE',  ( 141.1265829792455975, -3661.973233856808747, 2257.683488261172442 ) ) ;
#921 = ORIENTED_EDGE ( 'NONE', *, *, #10737, .F. ) ;
#922 = ORIENTED_EDGE ( 'NONE', *, *, #20905, .F. ) ;
#923 = VERTEX_POINT ( 'NONE', #16335 ) ;
#924 = DIRECTION ( 'NONE',  ( 0.000000000000000000, 0.000000000000000000, -1.000000000000000000 ) ) ;
#925 = VECTOR ( 'NONE', #12325, 1000.000000000000000 ) ;
#926 = B_SPLINE_CURVE_WITH_KNOTS ( 'NONE', 3,
 ( #9817, #18617, #7734, #4437, #20157, #11573, #11239, #17080, #4543, #792, #22125, #14886, #13456, #2457, #11348, #6204, #18387, #16964, #6323, #13223, #20489, #20371, #20269, #2337, #22014, #16621, #13113, #14991, #8073, #18843, #5872, #2562, #2785, #4208, #9931, #18720, #9601, #18498, #8187, #21907, #9709, #16848, #15220, #694, #7843, #15108, #22231 ),
 .UNSPECIFIED., .F., .F.,
 ( 4, 2, 2, 1, 1, 2, 2, 2, 2, 1, 1, 1, 1, 2, 2, 2, 2, 2, 1, 2, 2, 2, 2, 1, 1, 2, 2, 4 ),
 ( 0.000000000000000000, 0.1250000000146304913, 0.1875000000219457230, 0.2187500000256033528, 0.2343750000274318346, 0.2421875000283457424, 0.2500000000292596503, 0.3750000000440060766, 0.4375000000513063481, 0.4687500000549565393, 0.4843750000567812464, 0.4921875000575812731, 0.4960937500578705417, 0.4980468750579331028, 0.5000000000579956083, 0.5625000000547328849, 0.5937500000531019673, 0.6093750000522863974, 0.6171875000518064480, 0.6210937500514964738, 0.6250000000511864995, 0.6875000000439721592, 0.7187500000402435862, 0.7343750000383787446, 0.7421875000375531828, 0.7460937500370307118, 0.7500000000365082409, 1.000000000000000000 ),
 .UNSPECIFIED. ) ;
#927 = VECTOR ( 'NONE', #17929, 1000.000000000000000 ) ;
#928 = VERTEX_POINT ( 'NONE', #12699 ) ;
#929 = AXIS2_PLACEMENT_3D ( 'NONE', #20726, #4336, #20384 ) ;
#930 = DIRECTION ( 'NONE',  ( 0.000000000000000000, 0.000000000000000000, 1.000000000000000000 ) ) ;
#931 = CARTESIAN_POINT ( 'NONE',  ( 10.99145740650285319, -3577.220312686051329, 2249.716781721822827 ) ) ;
#932 = PERSON_AND_ORGANIZATION ( #5446, #1895 ) ;
#933 = CIRCLE ( 'NONE', #10292, 0.7620000000000000107 ) ;
#934 = CARTESIAN_POINT ( 'NONE',  ( 142.0761082949672982, -3581.059198188035680, 2249.196594758551328 ) ) ;
#935 = ORIENTED_EDGE ( 'NONE', *, *, #12718, .F. ) ;
#936 = FACE_OUTER_BOUND ( 'NONE', #977, .T. ) ;
#937 =( BOUNDED_CURVE ( )  B_SPLINE_CURVE ( 3, ( #23010, #5105, #1456, #12360 ),
 .UNSPECIFIED., .F., .T. ) 
 B_SPLINE_CURVE_WITH_KNOTS ( ( 4, 4 ),
 ( 1.570796327144186710, 3.141592653589829975 ),
 .UNSPECIFIED. ) 
 CURVE ( )  GEOMETRIC_REPRESENTATION_ITEM ( )  RATIONAL_B_SPLINE_CURVE ( ( 1.000000000000000000, 0.8047378542066848661, 0.8047378542066848661, 1.000000000000000000 ) ) 
 REPRESENTATION_ITEM ( '' )  );
#938 = CALENDAR_DATE ( 2026, 26, 10 ) ;
#939 = EDGE_CURVE ( 'NONE', #17172, #16346, #1530, .T. ) ;
#940 = DIRECTION ( 'NONE',  ( -1.000000000000000000, 0.000000000000000000, 0.000000000000000000 ) ) ;
#941 = LINE ( 'NONE', #22041, #7424 ) ;
#942 = ADVANCED_FACE ( 'NONE', ( #18087 ), #11055, .F. ) ;
#943 = CARTESIAN_POINT ( 'NONE',  ( 134.2700811556670999, -3657.722455772349349, 2245.892455863900068 ) ) ;
#944 = EDGE_CURVE ( 'NONE', #12459, #5100, #7542, .T. ) ;
#945 = CIRCLE ( 'NONE', #2107, 3.606800000000000228 ) ;
#946 = VERTEX_POINT ( 'NONE', #12588 ) ;
#947 = AXIS2_PLACEMENT_3D ( 'NONE', #9154, #360, #5985 ) ;
#948 = DIRECTION ( 'NONE',  ( 1.000000000000000000, 0.000000000000000000, 0.000000000000000000 ) ) ;
#949 = EDGE_LOOP ( 'NONE', ( #16333, #1362, #2481, #15726 ) ) ;
#950 = ORIENTED_EDGE ( 'NONE', *, *, #15391, .T. ) ;
#951 = CARTESIAN_POINT ( 'NONE',  ( 130.6067999999989979, -3670.300000000000182, 2239.009999999999764 ) ) ;
#952 = VERTEX_POINT ( 'NONE', #7431 ) ;
#953 = VECTOR ( 'NONE', #3074, 1000.000000000000114 ) ;
#954 = CARTESIAN_POINT ( 'NONE',  ( 139.6999999999999886, -3579.494999999999891, 2272.030000000000200 ) ) ;
#955 = DIRECTION ( 'NONE',  ( 0.000000000000000000, -1.000000000000000000, 0.000000000000000000 ) ) ;
#956 = EDGE_CURVE ( 'NONE', #5163, #4127, #15793, .T. ) ;
#957 = VERTEX_POINT ( 'NONE', #11176 ) ;
#958 = CARTESIAN_POINT ( 'NONE',  ( 7.179249868354160569, -3658.027629572277874, 2245.486160608427326 ) ) ;
#959 = DIRECTION ( 'NONE',  ( 0.000000000000000000, -2.336881798971000105E-14, 1.000000000000000000 ) ) ;
#960 = AXIS2_PLACEMENT_3D ( 'NONE', #3818, #7804, #11891 ) ;
#961 = AXIS2_PLACEMENT_3D ( 'NONE', #7228, #7453, #21861 ) ;
#962 = DIRECTION ( 'NONE',  ( -0.8660254037825932949, -0.5000000000031962211, 5.608020032303961777E-12 ) ) ;
#963 = PERSON_AND_ORGANIZATION ( #5446, #1895 ) ;
#964 = DIRECTION ( 'NONE',  ( 0.000000000000000000, -1.000000000000000000, 0.000000000000000000 ) ) ;
#965 = DIRECTION ( 'NONE',  ( 0.000000000000000000, 0.000000000000000000, 1.000000000000000000 ) ) ;
#966 = CIRCLE ( 'NONE', #14083, 6.349999999999855760 ) ;
#967 = ADVANCED_FACE ( 'NONE', ( #21497 ), #19739, .F. ) ;
#968 = DIRECTION ( 'NONE',  ( 1.000000000000000000, 0.000000000000000000, 0.000000000000000000 ) ) ;
#969 = EDGE_CURVE ( 'NONE', #12882, #7229, #14290, .T. ) ;
#970 = PLANE ( 'NONE',  #17126 ) ;
#971 = CIRCLE ( 'NONE', #15574, 0.7619999999999987894 ) ;
#972 = ADVANCED_FACE ( 'NONE', ( #509 ), #18315, .T. ) ;
#973 = ORIENTED_EDGE ( 'NONE', *, *, #14428, .F. ) ;
#974 = FACE_OUTER_BOUND ( 'NONE', #6628, .T. ) ;
#975 = ORIENTED_EDGE ( 'NONE', *, *, #21568, .T. ) ;
#976 = ADVANCED_FACE ( 'NONE', ( #7198 ), #21945, .T. ) ;
#977 = EDGE_LOOP ( 'NONE', ( #4447, #15868, #1564, #22394 ) ) ;
#978 = CARTESIAN_POINT ( 'NONE',  ( 141.5805787415576162, -3581.637520105196927, 2257.752117343301052 ) ) ;
#979 = CIRCLE ( 'NONE', #16695, 0.3809999999999993947 ) ;
#980 = CARTESIAN_POINT ( 'NONE',  ( 117.9067999999989951, -3594.099999999999909, 2260.600000000000364 ) ) ;
#981 = ORIENTED_EDGE ( 'NONE', *, *, #2428, .F. ) ;
#982 = VERTEX_POINT ( 'NONE', #17970 ) ;
#983 = CARTESIAN_POINT ( 'NONE',  ( 139.7000000000063835, -3576.802599999822633, 2239.167815367340609 ) ) ;
#984 = CARTESIAN_POINT ( 'NONE',  ( 12.70000000005999929, -3656.812599999999748, 2242.820000000000164 ) ) ;
#985 = TOROIDAL_SURFACE ( 'NONE', #6999, 3.606799999999999784, 0.7620000000000000107 ) ;
#986 = CARTESIAN_POINT ( 'NONE',  ( 11.18998458582999866, -3601.915631438000219, 2279.715722610000284 ) ) ;
#987 = ADVANCED_FACE ( 'NONE', ( #16214 ), #20275, .T. ) ;
#988 = EDGE_CURVE ( 'NONE', #6309, #16212, #2601, .T. ) ;
#989 = VECTOR ( 'NONE', #22563, 1000.000000000000000 ) ;
#990 = DIRECTION ( 'NONE',  ( 0.000000000000000000, -1.000000000000000000, 0.000000000000000000 ) ) ;
#991 = CARTESIAN_POINT ( 'NONE',  ( 12.70000000002640839, -3576.802599999929498, 2239.391000000000076 ) ) ;
#992 = FACE_OUTER_BOUND ( 'NONE', #6317, .T. ) ;
#993 = LINE ( 'NONE', #6058, #8747 ) ;
#994 = EDGE_LOOP ( 'NONE', ( #22383, #1983, #12504, #7454 ) ) ;
#995 = PERSON_AND_ORGANIZATION ( #5446, #1895 ) ;
#996 = DIRECTION ( 'NONE',  ( 0.000000000000000000, 0.000000000000000000, -1.000000000000000000 ) ) ;
#997 = AXIS2_PLACEMENT_3D ( 'NONE', #16654, #2817, #607 ) ;
#998 = DIRECTION ( 'NONE',  ( 0.000000000000000000, 0.000000000000000000, -1.000000000000000000 ) ) ;
#999 = CIRCLE ( 'NONE', #8125, 1.269999999999882334 ) ;
#1000 = FACE_BOUND ( 'NONE', #1086, .T. ) ;
#1001 = ORIENTED_EDGE ( 'NONE', *, *, #2789, .T. ) ;
#1002 = DIRECTION ( 'NONE',  ( 0.000000000000000000, 0.000000000000000000, 1.000000000000000000 ) ) ;
#1003 = AXIS2_PLACEMENT_3D ( 'NONE', #2063, #21859, #16238 ) ;
#1004 = PLANE ( 'NONE',  #9161 ) ;
#1005 = CARTESIAN_POINT ( 'NONE',  ( 144.5506343064713803, -3662.527019523321087, 2245.844349661943852 ) ) ;
#1006 = ORIENTED_EDGE ( 'NONE', *, *, #12155, .F. ) ;
#1007 = CARTESIAN_POINT ( 'NONE',  ( 105.2067999999999870, -3568.700000000000273, 2259.837999999999738 ) ) ;
#1008 = CARTESIAN_POINT ( 'NONE',  ( 14.17818779929573658, -3661.936027002551782, 2249.598227899164613 ) ) ;
#1009 = ORIENTED_EDGE ( 'NONE', *, *, #7436, .T. ) ;
#1010 = FACE_OUTER_BOUND ( 'NONE', #19730, .T. ) ;
#1011 = CYLINDRICAL_SURFACE ( 'NONE', #18913, 3.175000000000149925 ) ;
#1012 = CIRCLE ( 'NONE', #20868, 1.269999999999882334 ) ;
#1013 = DIRECTION ( 'NONE',  ( 0.000000000000000000, 0.000000000000000000, -1.000000000000000000 ) ) ;
#1014 = CARTESIAN_POINT ( 'NONE',  ( 11.18976463363000029, -3597.079503524999836, 2279.715692703000059 ) ) ;
#1015 = DIRECTION ( 'NONE',  ( 1.000000000000000000, 0.000000000000000000, 0.000000000000000000 ) ) ;
#1016 = ORIENTED_EDGE ( 'NONE', *, *, #14533, .F. ) ;
#1017 = ORIENTED_EDGE ( 'NONE', *, *, #3853, .F. ) ;
#1018 = AXIS2_PLACEMENT_3D ( 'NONE', #17663, #8653, #21200 ) ;
#1019 = AXIS2_PLACEMENT_3D ( 'NONE', #14450, #2022, #21597 ) ;
#1020 = DIRECTION ( 'NONE',  ( 0.8660254037820785955, -0.5000000000040877302, -3.181634500919918361E-14 ) ) ;
#1021 = ORIENTED_EDGE ( 'NONE', *, *, #18156, .F. ) ;
#1022 = CARTESIAN_POINT ( 'NONE',  ( 140.6228164679936867, -3656.807677064647578, 2257.629692242904184 ) ) ;
#1023 = DIRECTION ( 'NONE',  ( 0.000000000000000000, 0.000000000000000000, 1.000000000000000000 ) ) ;
#1024 = FACE_OUTER_BOUND ( 'NONE', #8988, .T. ) ;
#1025 = DIRECTION ( 'NONE',  ( 0.000000000000000000, 0.000000000000000000, 1.000000000000000000 ) ) ;
#1026 = APPLIED_PERSON_AND_ORGANIZATION_ASSIGNMENT ( #14097, #14334, ( #22796 ) ) ;
#1027 = CARTESIAN_POINT ( 'NONE',  ( 10.36831320284000135, -3638.156300000000101, 2292.781800000000203 ) ) ;
#1028 = VECTOR ( 'NONE', #2848, 1000.000000000000000 ) ;
#1029 = EDGE_CURVE ( 'NONE', #4102, #3301, #16883, .T. ) ;
#1030 = DIRECTION ( 'NONE',  ( -1.000000000000000000, 1.295098308110999804E-13, 2.590196616220999964E-13 ) ) ;
#1031 = ORIENTED_EDGE ( 'NONE', *, *, #1491, .F. ) ;
#1032 = CARTESIAN_POINT ( 'NONE',  ( 134.6199999999999761, -3579.494999999999891, 2239.009999999999764 ) ) ;
#1033 = AXIS2_PLACEMENT_3D ( 'NONE', #1523, #3286, #15281 ) ;
#1034 = EDGE_CURVE ( 'NONE', #2027, #9562, #13521, .T. ) ;
#1035 = CYLINDRICAL_SURFACE ( 'NONE', #23027, 0.3809999999999993947 ) ;
#1036 = ORIENTED_EDGE ( 'NONE', *, *, #20193, .F. ) ;
#1037 = EDGE_CURVE ( 'NONE', #19446, #15888, #18015, .T. ) ;
#1038 = LINE ( 'NONE', #10178, #18902 ) ;
#1039 = DIRECTION ( 'NONE',  ( 0.000000000000000000, 0.000000000000000000, -1.000000000000000000 ) ) ;
#1040 = ADVANCED_FACE ( 'NONE', ( #13493 ), #11393, .F. ) ;
#1041 = ORIENTED_EDGE ( 'NONE', *, *, #18117, .T. ) ;
#1042 = ORIENTED_EDGE ( 'NONE', *, *, #5637, .T. ) ;
#1043 = EDGE_LOOP ( 'NONE', ( #18572, #7602, #16545, #8314 ) ) ;
#1044 = VERTEX_POINT ( 'NONE', #13265 ) ;
#1045 = APPROVAL_ROLE ( '' ) ;
#1046 = LINE ( 'NONE', #6112, #6079 ) ;
#1047 = EDGE_LOOP ( 'NONE', ( #19998, #10354 ) ) ;
#1048 = AXIS2_PLACEMENT_3D ( 'NONE', #4123, #18073, #7418 ) ;
#1049 = DIRECTION ( 'NONE',  ( -1.000000000000000000, 0.000000000000000000, 0.000000000000000000 ) ) ;
#1050 = DIRECTION ( 'NONE',  ( 0.000000000000000000, -1.000000000000000000, 0.000000000000000000 ) ) ;
#1051 = DIRECTION ( 'NONE',  ( 1.000000000000000000, 0.000000000000000000, 0.000000000000000000 ) ) ;
#1052 = EDGE_CURVE ( 'NONE', #8155, #9937, #725, .T. ) ;
#1053 = CARTESIAN_POINT ( 'NONE',  ( 141.5833498427044788, -3581.627187199552282, 2248.052646821879534 ) ) ;
#1054 = ORIENTED_EDGE ( 'NONE', *, *, #11441, .T. ) ;
#1055 = CARTESIAN_POINT ( 'NONE',  ( 137.4378581446332532, -3581.229941748726105, 2257.824813627034928 ) ) ;
#1056 = SHAPE_DEFINITION_REPRESENTATION ( #8445, #9499 ) ;
#1057 = CARTESIAN_POINT ( 'NONE',  ( 3.810000000000000053, -3543.299999999999727, 2228.849999999999909 ) ) ;
#1058 = CARTESIAN_POINT ( 'NONE',  ( -5.588000000000000078, -3578.860000000000127, 2247.392000000000280 ) ) ;
#1059 = DIRECTION ( 'NONE',  ( 1.000000000000000000, 0.000000000000000000, 0.000000000000000000 ) ) ;
#1060 = EDGE_LOOP ( 'NONE', ( #18493, #3265, #9177, #20346 ) ) ;
#1061 = CARTESIAN_POINT ( 'NONE',  ( 142.4730284656999970, -3660.140000970000074, 2250.236800000000130 ) ) ;
#1062 = ORIENTED_EDGE ( 'NONE', *, *, #14592, .T. ) ;
#1063 = AXIS2_PLACEMENT_3D ( 'NONE', #9805, #5967, #12995 ) ;
#1064 = DIRECTION ( 'NONE',  ( -2.318894227180156550E-14, -1.000000000000000000, 0.000000000000000000 ) ) ;
#1065 = EDGE_CURVE ( 'NONE', #15615, #6279, #20636, .T. ) ;
#1066 = ADVANCED_FACE ( 'NONE', ( #11734 ), #9746, .T. ) ;
#1067 = CARTESIAN_POINT ( 'NONE',  ( 139.6999999999999886, -3579.494999999999891, 2245.359999999999673 ) ) ;
#1068 = ORIENTED_EDGE ( 'NONE', *, *, #5816, .T. ) ;
#1069 = ORIENTED_EDGE ( 'NONE', *, *, #7661, .F. ) ;
#1070 = DIRECTION ( 'NONE',  ( 0.000000000000000000, 1.000000000000000000, 0.000000000000000000 ) ) ;
#1071 = FACE_OUTER_BOUND ( 'NONE', #18282, .T. ) ;
#1072 = ORIENTED_EDGE ( 'NONE', *, *, #10277, .F. ) ;
#1073 = DIRECTION ( 'NONE',  ( -1.000000000000000000, 0.000000000000000000, 0.000000000000000000 ) ) ;
#1074 = CARTESIAN_POINT ( 'NONE',  ( 137.1599999999999966, -3544.570000000000164, 2255.774000000000342 ) ) ;
#1075 = DIRECTION ( 'NONE',  ( 0.000000000000000000, 0.000000000000000000, -1.000000000000000000 ) ) ;
#1076 = PERSON_AND_ORGANIZATION ( #5446, #1895 ) ;
#1077 = CARTESIAN_POINT ( 'NONE',  ( 137.3683132029851208, -3660.851200000049630, 2239.391000000000076 ) ) ;
#1078 = DIRECTION ( 'NONE',  ( -2.324635735433000053E-14, 0.000000000000000000, -1.000000000000000000 ) ) ;
#1079 = DIRECTION ( 'NONE',  ( 0.000000000000000000, 0.000000000000000000, 1.000000000000000000 ) ) ;
#1080 = EDGE_CURVE ( 'NONE', #9518, #22946, #12776, .T. ) ;
#1081 = AXIS2_PLACEMENT_3D ( 'NONE', #4745, #21035, #19158 ) ;
#1082 = CARTESIAN_POINT ( 'NONE',  ( 141.9222097098283371, -3657.728223441102273, 2248.902296121618747 ) ) ;
#1083 = CARTESIAN_POINT ( 'NONE',  ( 35.56000000000000227, -3694.430000000000291, 2251.506800000000112 ) ) ;
#1084 = ORIENTED_EDGE ( 'NONE', *, *, #8969, .F. ) ;
#1085 = CARTESIAN_POINT ( 'NONE',  ( 9.987313202835000681, -3637.936329547000241, 2296.591799999999694 ) ) ;
#1086 = EDGE_LOOP ( 'NONE', ( #1869, #15862 ) ) ;
#1087 = ORIENTED_EDGE ( 'NONE', *, *, #5302, .F. ) ;
#1088 = CARTESIAN_POINT ( 'NONE',  ( 2.859369265564648099, -3695.699999999999818, 2275.763800000091578 ) ) ;
#1089 = CIRCLE ( 'NONE', #359, 4.114799999999974034 ) ;
#1090 = DIRECTION ( 'NONE',  ( 2.324635735433000053E-14, 0.000000000000000000, 1.000000000000000000 ) ) ;
#1091 = ORIENTED_EDGE ( 'NONE', *, *, #12878, .T. ) ;
#1092 = VERTEX_POINT ( 'NONE', #9978 ) ;
#1093 = APPLIED_APPROVAL_ASSIGNMENT ( #15222, ( #13135 ) ) ;
#1094 = PLANE ( 'NONE',  #3530 ) ;
#1095 = AXIS2_PLACEMENT_3D ( 'NONE', #16221, #14126, #21385 ) ;
#1096 = CARTESIAN_POINT ( 'NONE',  ( 10.46820691843999995, -3601.271459550000145, 2279.591867610000008 ) ) ;
#1097 = EDGE_CURVE ( 'NONE', #7706, #11149, #20418, .T. ) ;
#1098 = EDGE_LOOP ( 'NONE', ( #981, #7188, #17231, #14230, #4142, #11385 ) ) ;
#1099 = EDGE_CURVE ( 'NONE', #11125, #20633, #16892, .T. ) ;
#1100 = DIRECTION ( 'NONE',  ( 0.000000000000000000, 0.000000000000000000, 1.000000000000000000 ) ) ;
#1101 = CARTESIAN_POINT ( 'NONE',  ( 15.03168679714000078, -3600.843699999999899, 2292.781800000000203 ) ) ;
#1102 = EDGE_CURVE ( 'NONE', #19933, #2928, #6479, .T. ) ;
#1103 = DIRECTION ( 'NONE',  ( 0.8660254037840939834, -0.5000000000005969669, 0.000000000000000000 ) ) ;
#1104 = CARTESIAN_POINT ( 'NONE',  ( 15.03168679714165634, -3598.151299999852654, 2296.433984632644751 ) ) ;
#1105 = ORIENTED_EDGE ( 'NONE', *, *, #10084, .F. ) ;
#1106 = CALENDAR_DATE ( 2026, 26, 10 ) ;
#1107 = DIRECTION ( 'NONE',  ( 0.000000000000000000, -2.331176954594000018E-14, 1.000000000000000000 ) ) ;
#1108 = EDGE_CURVE ( 'NONE', #10881, #6183, #10904, .T. ) ;
#1109 = AXIS2_PLACEMENT_3D ( 'NONE', #7606, #2336, #580 ) ;
#1110 = CARTESIAN_POINT ( 'NONE',  ( 10.19827476683941825, -3580.849530610950296, 2249.426096155833875 ) ) ;
#1111 = DIRECTION ( 'NONE',  ( 0.000000000000000000, -1.000000000000000000, 0.000000000000000000 ) ) ;
#1112 = APPLIED_SECURITY_CLASSIFICATION_ASSIGNMENT ( #381, ( #11230 ) ) ;
#1113 = ORIENTED_EDGE ( 'NONE', *, *, #6592, .T. ) ;
#1114 = ADVANCED_FACE ( 'NONE', ( #4472 ), #22052, .T. ) ;
#1115 = CARTESIAN_POINT ( 'NONE',  ( -12.69999999999997087, -3577.293829547214045, 2250.104686797002159 ) ) ;
#1116 = EDGE_CURVE ( 'NONE', #20178, #4557, #4253, .T. ) ;
#1117 = FACE_OUTER_BOUND ( 'NONE', #19737, .T. ) ;
#1118 = CARTESIAN_POINT ( 'NONE',  ( 144.9133339346259390, -3661.846445636756471, 2245.115832528513693 ) ) ;
#1119 = DIRECTION ( 'NONE',  ( 0.000000000000000000, -1.000000000000000000, 0.000000000000000000 ) ) ;
#1120 = DIRECTION ( 'NONE',  ( 0.000000000000000000, 1.000000000000000000, 0.000000000000000000 ) ) ;
#1121 = FACE_OUTER_BOUND ( 'NONE', #15842, .T. ) ;
#1122 = VERTEX_POINT ( 'NONE', #15267 ) ;
#1123 = CARTESIAN_POINT ( 'NONE',  ( 10.36831320285999958, -3580.841199999999844, 2242.820000000000164 ) ) ;
#1124 = DIRECTION ( 'NONE',  ( 0.000000000000000000, 0.000000000000000000, -1.000000000000000000 ) ) ;
#1125 = VECTOR ( 'NONE', #6435, 1000.000000000000000 ) ;
#1126 = ADVANCED_FACE ( 'NONE', ( #2713 ), #22166, .F. ) ;
#1127 = CARTESIAN_POINT ( 'NONE',  ( 136.8551930557000276, -3659.505009668000184, 2250.165028799000083 ) ) ;
#1128 = CARTESIAN_POINT ( 'NONE',  ( 134.3871257470999865, -3581.600847139000052, 2246.630000000000109 ) ) ;
#1129 = DIRECTION ( 'NONE',  ( 0.000000000000000000, 0.000000000000000000, 1.000000000000000000 ) ) ;
#1130 = ORGANIZATION ( 'NAUO-ORG1', 'UNSPECIFIED', 'UNSPECIFIED' ) ;
#1131 = B_SPLINE_CURVE_WITH_KNOTS ( 'NONE', 3,
 ( #7869, #8105, #7758, #18748, #9623, #15249, #4573, #11716, #18869, #4118, #18411, #2814, #22148, #11264, #18640, #14790, #21928, #11489 ),
 .UNSPECIFIED., .F., .F.,
 ( 4, 2, 2, 2, 2, 2, 2, 2, 4 ),
 ( 0.008925482226561637714, 0.009483346987770943301, 0.01004121174898024715, 0.01059907651018955274, 0.01115694127139885833, 0.01171480603260816218, 0.01227267079381746777, 0.01283053555502677162, 0.01338840031623607721 ),
 .UNSPECIFIED. ) ;
#1132 = APPLIED_APPROVAL_ASSIGNMENT ( #889, ( #17087 ) ) ;
#1133 = ORIENTED_EDGE ( 'NONE', *, *, #2952, .T. ) ;
#1134 = VECTOR ( 'NONE', #15380, 1000.000000000000000 ) ;
#1135 = CARTESIAN_POINT ( 'NONE',  ( 10.36831320289432057, -3600.843700000111312, 2296.210799999999836 ) ) ;
#1136 = ORIENTED_EDGE ( 'NONE', *, *, #9565, .T. ) ;
#1137 = CARTESIAN_POINT ( 'NONE',  ( 14.27720943205999937, -3581.868154638000306, 2257.704281108000032 ) ) ;
#1138 = PERSON_AND_ORGANIZATION_ROLE ( 'classification_officer' ) ;
#1139 = DIRECTION ( 'NONE',  ( -1.000000000000000000, 0.000000000000000000, 0.000000000000000000 ) ) ;
#1140 = CARTESIAN_POINT ( 'NONE',  ( 142.2556445848496480, -3578.231573646348352, 2257.890254708840530 ) ) ;
#1141 = DIRECTION ( 'NONE',  ( -2.324635735433000053E-14, 0.000000000000000000, -1.000000000000000000 ) ) ;
#1142 = CYLINDRICAL_SURFACE ( 'NONE', #15235, 5.460999999999938126 ) ;
#1143 = CYLINDRICAL_SURFACE ( 'NONE', #10596, 5.714999999999999858 ) ;
#1144 = LOCAL_TIME ( 17, 37, 43.00000000000000000, #14164 ) ;
#1145 = CARTESIAN_POINT ( 'NONE',  ( 137.2727299238133583, -3578.011210012966785, 2250.107278179072637 ) ) ;
#1146 = ORIENTED_EDGE ( 'NONE', *, *, #19120, .T. ) ;
#1147 = APPLIED_SECURITY_CLASSIFICATION_ASSIGNMENT ( #6402, ( #20249 ) ) ;
#1148 = CARTESIAN_POINT ( 'NONE',  ( 1.270000000000000018, -3543.299999999999727, 2240.279999999999745 ) ) ;
#1149 = DIRECTION ( 'NONE',  ( 1.000000000000000000, 0.000000000000000000, 0.000000000000000000 ) ) ;
#1150 = VERTEX_POINT ( 'NONE', #6255 ) ;
#1151 = DIRECTION ( 'NONE',  ( -0.6887494619146010688, 0.000000000000000000, 0.7249994335945012525 ) ) ;
#1152 = CARTESIAN_POINT ( 'NONE',  ( 10.13128874078853414, -3658.282160798511995, 2249.547058791628388 ) ) ;
#1153 = ORIENTED_EDGE ( 'NONE', *, *, #16561, .T. ) ;
#1154 = CIRCLE ( 'NONE', #16503, 3.606799999999993567 ) ;
#1155 = ORIENTED_EDGE ( 'NONE', *, *, #14885, .F. ) ;
#1156 = CARTESIAN_POINT ( 'NONE',  ( 134.1795861059526374, -3580.969250050632581, 2245.481136081417844 ) ) ;
#1157 = EDGE_LOOP ( 'NONE', ( #19411, #15979, #3547, #7427 ) ) ;
#1158 = APPLIED_DATE_AND_TIME_ASSIGNMENT ( #13724, #15358, ( #3363 ) ) ;
#1159 = CARTESIAN_POINT ( 'NONE',  ( 29.00679999999900005, -3568.700000000000273, 2259.837999999999738 ) ) ;
#1160 = CARTESIAN_POINT ( 'NONE',  ( -6.349999999999999645, -3578.860000000000127, 2247.392000000000280 ) ) ;
#1161 = CARTESIAN_POINT ( 'NONE',  ( 141.6023748289098592, -3581.610180818415756, 2248.119666950691226 ) ) ;
#1162 = ORIENTED_EDGE ( 'NONE', *, *, #20568, .T. ) ;
#1163 = DIRECTION ( 'NONE',  ( 0.8660254037840939834, -0.5000000000005969669, 0.000000000000000000 ) ) ;
#1164 = CALENDAR_DATE ( 2026, 26, 10 ) ;
#1165 = ADVANCED_FACE ( 'NONE', ( #11612 ), #6827, .T. ) ;
#1166 = DIRECTION ( 'NONE',  ( 0.8660254037816507156, 0.5000000000048288040, 0.000000000000000000 ) ) ;
#1167 = CARTESIAN_POINT ( 'NONE',  ( 14.58530482363100766, -3581.625685692691150, 2248.064425038887748 ) ) ;
#1168 = TOROIDAL_SURFACE ( 'NONE', #14289, 7.112000000000000099, 0.7620000000000000107 ) ;
#1169 = EDGE_CURVE ( 'NONE', #18991, #7862, #5466, .T. ) ;
#1170 = DIRECTION ( 'NONE',  ( 0.000000000000000000, 1.000000000000000000, 0.000000000000000000 ) ) ;
#1171 = AXIS2_PLACEMENT_3D ( 'NONE', #4369, #8003, #15148 ) ;
#1172 = ORIENTED_EDGE ( 'NONE', *, *, #5841, .F. ) ;
#1173 = CARTESIAN_POINT ( 'NONE',  ( 0.000000000000000000, -3694.430000000000291, 2254.503999999999905 ) ) ;
#1174 = DIRECTION ( 'NONE',  ( -1.000000000000000000, 0.000000000000000000, 0.000000000000000000 ) ) ;
#1175 = ORIENTED_EDGE ( 'NONE', *, *, #1982, .F. ) ;
#1176 = DIRECTION ( 'NONE',  ( 0.000000000000000000, -1.000000000000000000, 0.000000000000000000 ) ) ;
#1177 = CARTESIAN_POINT ( 'NONE',  ( 12.69999999999999929, -3599.497499999999945, 2288.971800000000258 ) ) ;
#1178 = ORIENTED_EDGE ( 'NONE', *, *, #4955, .T. ) ;
#1179 = ORIENTED_EDGE ( 'NONE', *, *, #15365, .T. ) ;
#1180 = CARTESIAN_POINT ( 'NONE',  ( 151.1299999999999955, -3694.430000000000291, 2239.009999999999764 ) ) ;
#1181 = CARTESIAN_POINT ( 'NONE',  ( 134.0175234625681639, -3660.113920206924831, 2244.547288873641264 ) ) ;
#1182 = VECTOR ( 'NONE', #22756, 1000.000000000000000 ) ;
#1183 = ORIENTED_EDGE ( 'NONE', *, *, #18454, .T. ) ;
#1184 = APPLIED_PERSON_AND_ORGANIZATION_ASSIGNMENT ( #23012, #3452, ( #20249 ) ) ;
#1185 = CIRCLE ( 'NONE', #9064, 3.606799999998994366 ) ;
#1186 = CARTESIAN_POINT ( 'NONE',  ( 12.69999999999999929, -3634.041499999999814, 2296.210799999999836 ) ) ;
#1187 = LINE ( 'NONE', #6483, #14984 ) ;
#1188 = CARTESIAN_POINT ( 'NONE',  ( 12.70000000000085194, -3602.342301254449922, 2279.817638608976267 ) ) ;
#1189 = DIRECTION ( 'NONE',  ( -0.8660254037842058938, -0.5000000000004030110, 0.000000000000000000 ) ) ;
#1190 = PERSON_AND_ORGANIZATION ( #5446, #1895 ) ;
#1191 = EDGE_CURVE ( 'NONE', #6461, #15432, #8756, .T. ) ;
#1192 = CARTESIAN_POINT ( 'NONE',  ( 0.000000000000000000, -3695.699999999999818, 2260.600000000000364 ) ) ;
#1193 = DIRECTION ( 'NONE',  ( 0.000000000000000000, 0.000000000000000000, -1.000000000000000000 ) ) ;
#1195 = EDGE_CURVE ( 'NONE', #5090, #6776, #8349, .T. ) ;
#1194 = DIRECTION ( 'NONE',  ( 0.000000000000000000, 0.000000000000000000, -1.000000000000000000 ) ) ;
#1196 = CIRCLE ( 'NONE', #13926, 3.606799999999993567 ) ;
#1197 = EDGE_CURVE ( 'NONE', #9068, #1906, #14089, .T. ) ;
#1198 = CARTESIAN_POINT ( 'NONE',  ( 141.9794657906317070, -3657.802918816917099, 2249.014193234177128 ) ) ;
#1199 = AXIS2_PLACEMENT_3D ( 'NONE', #4778, #19071, #10279 ) ;
#1200 = VERTEX_POINT ( 'NONE', #8469 ) ;
#1201 = VECTOR ( 'NONE', #1139, 1000.000000000000000 ) ;
#1202 = CARTESIAN_POINT ( 'NONE',  ( 123.3932000000010021, -3670.300000000000182, 2239.009999999999764 ) ) ;
#1203 = CIRCLE ( 'NONE', #2699, 2.844799999998998796 ) ;
#1204 = ADVANCED_FACE ( 'NONE', ( #13742 ), #20887, .T. ) ;
#1205 = VERTEX_POINT ( 'NONE', #3299 ) ;
#1206 = CARTESIAN_POINT ( 'NONE',  ( 10.06338274650999942, -3580.575356121999903, 2257.909778189000008 ) ) ;
#1207 = DIRECTION ( 'NONE',  ( 0.000000000000000000, 1.000000000000000000, 0.000000000000000000 ) ) ;
#1208 = ORIENTED_EDGE ( 'NONE', *, *, #17127, .F. ) ;
#1209 = ORIENTED_EDGE ( 'NONE', *, *, #9849, .T. ) ;
#1210 = CARTESIAN_POINT ( 'NONE',  ( -5.588000000000000078, -3543.299999999999727, 2229.612000000000080 ) ) ;
#1211 = ADVANCED_FACE ( 'NONE', ( #4941 ), #19241, .F. ) ;
#1212 = CARTESIAN_POINT ( 'NONE',  ( 12.70000000002640839, -3656.812599999929262, 2239.391000000000076 ) ) ;
#1213 = AXIS2_PLACEMENT_3D ( 'NONE', #22153, #5785, #14682 ) ;
#1214 = CARTESIAN_POINT ( 'NONE',  ( 151.1299999999999955, -3694.430000000000291, 2259.329999999999927 ) ) ;
#1215 = ORIENTED_EDGE ( 'NONE', *, *, #418, .T. ) ;
#1216 = CARTESIAN_POINT ( 'NONE',  ( 97.99320000000000164, -3619.500000000000000, 2239.771999999999935 ) ) ;
#1217 = DIRECTION ( 'NONE',  ( 4.097771990502999700E-13, -2.590196616219000170E-13, -1.000000000000000000 ) ) ;
#1218 = CARTESIAN_POINT ( 'NONE',  ( -5.588000000000000078, -3543.299999999999727, 2253.487999999999829 ) ) ;
#1219 = CARTESIAN_POINT ( 'NONE',  ( 64.76999999999999602, -3670.300000000000182, 2286.368300000000090 ) ) ;
#1220 = VECTOR ( 'NONE', #22541, 1000.000000000000000 ) ;
#1221 = FACE_OUTER_BOUND ( 'NONE', #1060, .T. ) ;
#1222 = ORIENTED_EDGE ( 'NONE', *, *, #2628, .T. ) ;
#1223 = PERSON_AND_ORGANIZATION_ROLE ( 'creator' ) ;
#1224 = AXIS2_PLACEMENT_3D ( 'NONE', #10858, #14615, #21755 ) ;
#1225 = APPLICATION_CONTEXT ( 'configuration controlled 3d designs of mechanical parts and assemblies' ) ;
#1226 = ORIENTED_EDGE ( 'NONE', *, *, #19841, .T. ) ;
#1227 = DIRECTION ( 'NONE',  ( 0.000000000000000000, 1.000000000000000000, 0.000000000000000000 ) ) ;
#1228 = ADVANCED_FACE ( 'NONE', ( #3414 ), #15843, .T. ) ;
#1229 = CARTESIAN_POINT ( 'NONE',  ( 10.58917828235573921, -3581.402186961769075, 2248.668793006535452 ) ) ;
#1230 = CARTESIAN_POINT ( 'NONE',  ( 9.879064962501331593, -3659.930690980918371, 2250.236800000000130 ) ) ;
#1231 = ADVANCED_BREP_SHAPE_REPRESENTATION ( '', ( #21284, #5611 ), #12740 ) ;
#1232 = VERTEX_POINT ( 'NONE', #15961 ) ;
#1233 = TOROIDAL_SURFACE ( 'NONE', #14719, 5.080000000000000071, 0.3810000000000000053 ) ;
#1234 = FACE_OUTER_BOUND ( 'NONE', #3100, .T. ) ;
#1235 = EDGE_CURVE ( 'NONE', #14115, #3220, #6064, .T. ) ;
#1236 = EDGE_CURVE ( 'NONE', #3458, #17328, #6429, .T. ) ;
#1237 = FACE_OUTER_BOUND ( 'NONE', #16909, .T. ) ;
#1238 = CARTESIAN_POINT ( 'NONE',  ( 145.2534987145345440, -3660.862304053093339, 2244.636253111490532 ) ) ;
#1239 = AXIS2_PLACEMENT_3D ( 'NONE', #15381, #9530, #20423 ) ;
#1240 = DIRECTION ( 'NONE',  ( -0.8660254037840939834, -0.5000000000005969669, 0.000000000000000000 ) ) ;
#1241 = CARTESIAN_POINT ( 'NONE',  ( 11.45794194510839681, -3662.064378513683096, 2249.487216201922820 ) ) ;
#1242 = CIRCLE ( 'NONE', #12846, 3.606799999999993567 ) ;
#1243 = ORIENTED_EDGE ( 'NONE', *, *, #16662, .T. ) ;
#1244 = CARTESIAN_POINT ( 'NONE',  ( 151.1299999999999955, -3695.699999999999818, 2259.329999999999927 ) ) ;
#1245 = DIRECTION ( 'NONE',  ( 1.000000000000000000, -2.330758767201999921E-14, -2.339144844575000061E-14 ) ) ;
#1246 = CARTESIAN_POINT ( 'NONE',  ( 7.387125747139000609, -3581.600847139000052, 2246.630000000000109 ) ) ;
#1247 = CARTESIAN_POINT ( 'NONE',  ( 139.6999999999999886, -3662.637340904999746, 2239.009999999999764 ) ) ;
#1248 = LINE ( 'NONE', #9918, #11318 ) ;
#1249 = ADVANCED_FACE ( 'NONE', ( #5064 ), #11632, .T. ) ;
#1250 = ORIENTED_EDGE ( 'NONE', *, *, #12458, .F. ) ;
#1251 = CARTESIAN_POINT ( 'NONE',  ( 6.985153502415999860, -3659.505556594000154, 2244.618656866000038 ) ) ;
#1252 = VERTEX_POINT ( 'NONE', #1180 ) ;
#1253 = CARTESIAN_POINT ( 'NONE',  ( 1.270000000000000018, -3544.570000000000164, 2239.009999999999764 ) ) ;
#1254 = CALENDAR_DATE ( 2026, 26, 10 ) ;
#1255 = APPLICATION_CONTEXT ( 'configuration controlled 3d designs of mechanical parts and assemblies' ) ;
#1256 = DIRECTION ( 'NONE',  ( 0.000000000000000000, 0.000000000000000000, -1.000000000000000000 ) ) ;
#1257 = DIRECTION ( 'NONE',  ( 0.000000000000000000, 0.000000000000000000, -1.000000000000000000 ) ) ;
#1258 = CARTESIAN_POINT ( 'NONE',  ( 12.70000020906999971, -3662.349800009999854, 2257.592639999999847 ) ) ;
#1259 = DIRECTION ( 'NONE',  ( -1.000000000000000000, 0.000000000000000000, 0.000000000000000000 ) ) ;
#1260 = CYLINDRICAL_SURFACE ( 'NONE', #5745, 2.844799999999994444 ) ;
#1261 = ADVANCED_FACE ( 'NONE', ( #17474 ), #5308, .T. ) ;
#1262 = DIRECTION ( 'NONE',  ( -1.000000000000000000, 0.000000000000000000, 0.000000000000000000 ) ) ;
#1263 = B_SPLINE_CURVE_WITH_KNOTS ( 'NONE', 3,
 ( #22636, #8483, #10342, #17489, #22757, #8591, #6843, #13983, #12223, #10459, #19372, #3309, #17602, #8707, #22985, #5429, #21600, #17953, #7525, #154, #5784, #2025, #10809, #16542, #5556, #14453, #9295, #7185, #12915, #9407, #16316, #382, #20184, #7635, #3893, #9175, #1903, #495, #12687, #19835, #16428 ),
 .UNSPECIFIED., .F., .F.,
 ( 4, 2, 2, 1, 1, 2, 2, 2, 2, 1, 1, 1, 2, 2, 2, 2, 2, 2, 2, 1, 1, 2, 2, 4 ),
 ( 0.000000000000000000, 0.1249999999979331533, 0.1874999999971100062, 0.2187499999967864872, 0.2343749999967179587, 0.2421874999969684528, 0.2499999999972189468, 0.3750000000075985329, 0.4375000000129096733, 0.4687500000155650492, 0.4843750000170347070, 0.4921875000177692860, 0.4960937500180022108, 0.5000000000182350801, 0.5625000000188430382, 0.5937500000189966931, 0.6250000000191502370, 0.6875000000194086969, 0.7187500000195379268, 0.7343750000196028749, 0.7421875000200089945, 0.7460937500199683603, 0.7500000000199277261, 1.000000000000000000 ),
 .UNSPECIFIED. ) ;
#1264 = ORIENTED_EDGE ( 'NONE', *, *, #19451, .F. ) ;
#1265 = AXIS2_PLACEMENT_3D ( 'NONE', #6682, #19325, #16038 ) ;
#1266 = CARTESIAN_POINT ( 'NONE',  ( 15.03168679716000078, -3575.456400000000031, 2242.820000000000164 ) ) ;
#1267 = DIRECTION ( 'NONE',  ( 0.000000000000000000, 0.000000000000000000, 1.000000000000000000 ) ) ;
#1268 = AXIS2_PLACEMENT_3D ( 'NONE', #17644, #3353, #21409 ) ;
#1269 = ORIENTED_EDGE ( 'NONE', *, *, #2702, .F. ) ;
#1270 = DIRECTION ( 'NONE',  ( 0.000000000000000000, 0.000000000000000000, -1.000000000000000000 ) ) ;
#1271 = CARTESIAN_POINT ( 'NONE',  ( 9.916981607687798572, -3658.814059329320116, 2249.942683905858303 ) ) ;
#1272 = ORIENTED_EDGE ( 'NONE', *, *, #10390, .F. ) ;
#1273 = ORIENTED_EDGE ( 'NONE', *, *, #7526, .T. ) ;
#1274 = DIRECTION ( 'NONE',  ( -0.000000000000000000, 1.000000000000000000, 0.000000000000000000 ) ) ;
#1275 = PRODUCT_DEFINITION_CONTEXT ( 'detailed design', #14590, 'design' ) ;
#1276 =( BOUNDED_CURVE ( )  B_SPLINE_CURVE ( 3, ( #21761, #18012, #11101, #435 ),
 .UNSPECIFIED., .F., .T. ) 
 B_SPLINE_CURVE_WITH_KNOTS ( ( 4, 4 ),
 ( -8.881784197001252323E-16, 1.570796326722519565 ),
 .UNSPECIFIED. ) 
 CURVE ( )  GEOMETRIC_REPRESENTATION_ITEM ( )  RATIONAL_B_SPLINE_CURVE ( ( 1.000000000000000000, 0.8047378541414241804, 0.8047378541414241804, 1.000000000000000000 ) ) 
 REPRESENTATION_ITEM ( '' )  );
#1277 = EDGE_CURVE ( 'NONE', #8369, #18910, #16516, .T. ) ;
#1278 = ORIENTED_EDGE ( 'NONE', *, *, #4244, .T. ) ;
#1279 = CARTESIAN_POINT ( 'NONE',  ( 18.37893127878000143, -3660.140301727999940, 2244.547200027999679 ) ) ;
#1280 = CARTESIAN_POINT ( 'NONE',  ( 0.000000000000000000, 0.000000000000000000, 0.000000000000000000 ) ) ;
#1281 = DIRECTION ( 'NONE',  ( 0.000000000000000000, 1.000000000000000000, 0.000000000000000000 ) ) ;
#1282 = ORIENTED_EDGE ( 'NONE', *, *, #9851, .T. ) ;
#1283 = CYLINDRICAL_SURFACE ( 'NONE', #8511, 0.3809999999999154618 ) ;
#1284 = VECTOR ( 'NONE', #17170, 1000.000000000000000 ) ;
#1285 = PERSON_AND_ORGANIZATION ( #5446, #1895 ) ;
#1286 = VECTOR ( 'NONE', #7795, 1000.000000000000000 ) ;
#1287 = AXIS2_PLACEMENT_3D ( 'NONE', #5797, #5569, #16104 ) ;
#1288 = FACE_OUTER_BOUND ( 'NONE', #22159, .T. ) ;
#1289 = DIRECTION ( 'NONE',  ( 0.000000000000000000, 0.000000000000000000, 1.000000000000000000 ) ) ;
#1290 = CARTESIAN_POINT ( 'NONE',  ( 134.1335424281758435, -3658.210520966862987, 2245.301510576022338 ) ) ;
#1291 = DIRECTION ( 'NONE',  ( -1.000000000000000000, 0.000000000000000000, 0.000000000000000000 ) ) ;
#1292 = EDGE_LOOP ( 'NONE', ( #10333, #22643, #21659, #2923 ) ) ;
#1293 = CARTESIAN_POINT ( 'NONE',  ( 12.69999999999999929, -3639.502500000000055, 2290.622800000000097 ) ) ;
#1294 = APPLIED_DATE_AND_TIME_ASSIGNMENT ( #5678, #2038, ( #9761 ) ) ;
#1295 = FACE_OUTER_BOUND ( 'NONE', #3645, .T. ) ;
#1296 = EDGE_LOOP ( 'NONE', ( #17068, #11898, #4290, #1902 ) ) ;
#1297 = CARTESIAN_POINT ( 'NONE',  ( 127.0000000000000000, -3568.700000000000273, 2259.837999999999738 ) ) ;
#1298 = VECTOR ( 'NONE', #9093, 1000.000000000000000 ) ;
#1299 = CIRCLE ( 'NONE', #3937, 1.269999999999993356 ) ;
#1300 = FACE_OUTER_BOUND ( 'NONE', #22874, .T. ) ;
#1301 = VECTOR ( 'NONE', #7650, 1000.000000000000000 ) ;
#1302 = ORIENTED_EDGE ( 'NONE', *, *, #2789, .F. ) ;
#1303 = CARTESIAN_POINT ( 'NONE',  ( 139.6999999999985675, -3582.369629489782255, 2239.009999999944739 ) ) ;
#1304 = DIRECTION ( 'NONE',  ( 0.000000000000000000, 1.000000000000000000, 0.000000000000000000 ) ) ;
#1305 = ORIENTED_EDGE ( 'NONE', *, *, #6122, .F. ) ;
#1306 = DIRECTION ( 'NONE',  ( 0.000000000000000000, 0.000000000000000000, 1.000000000000000000 ) ) ;
#1307 = CARTESIAN_POINT ( 'NONE',  ( 3.048000000000000043, -3543.299999999999727, 2238.248000000000047 ) ) ;
#1308 = CARTESIAN_POINT ( 'NONE',  ( 104.4447999999999865, -3670.300000000000182, 2261.869999999999891 ) ) ;
#1309 = CYLINDRICAL_SURFACE ( 'NONE', #15983, 2.844800000000091700 ) ;
#1310 = PERSON_AND_ORGANIZATION_ROLE ( 'classification_officer' ) ;
#1311 = DIRECTION ( 'NONE',  ( 5.572969907074833723E-14, -1.000000000000000000, 0.000000000000000000 ) ) ;
#1312 = CARTESIAN_POINT ( 'NONE',  ( 95.25000000000000000, -3544.570000000000164, 2251.506800000000112 ) ) ;
#1313 = CARTESIAN_POINT ( 'NONE',  ( 114.2999999999999972, -3594.099999999999909, 2260.600000000000364 ) ) ;
#1314 = AXIS2_PLACEMENT_3D ( 'NONE', #4707, #20997, #12205 ) ;
#1315 = TOROIDAL_SURFACE ( 'NONE', #18169, 5.080000000000000071, 0.3810000000000000053 ) ;
#1316 = PRODUCT_DEFINITION_SHAPE ( 'NONE', 'NONE',  #20503 ) ;
#1317 = CARTESIAN_POINT ( 'NONE',  ( 141.8962106656137223, -3657.696406372347610, 2248.849616286249784 ) ) ;
#1318 = CIRCLE ( 'NONE', #23015, 1.269999999999882334 ) ;
#1319 = ORIENTED_EDGE ( 'NONE', *, *, #10226, .T. ) ;
#1320 = AXIS2_PLACEMENT_3D ( 'NONE', #13380, #12199, #15718 ) ;
#1321 = CARTESIAN_POINT ( 'NONE',  ( 22.00181536726000076, -3694.938000000000102, 2275.224984633000076 ) ) ;
#1322 = APPROVAL ( #4119, 'UNSPECIFIED' ) ;
#1323 = ORIENTED_EDGE ( 'NONE', *, *, #19679, .F. ) ;
#1324 = DIRECTION ( 'NONE',  ( 1.000000000000000000, 0.000000000000000000, 0.000000000000000000 ) ) ;
#1325 = ADVANCED_FACE ( 'NONE', ( #21119 ), #14206, .F. ) ;
#1326 = ORIENTED_EDGE ( 'NONE', *, *, #6161, .T. ) ;
#1327 = ORIENTED_EDGE ( 'NONE', *, *, #3052, .T. ) ;
#1328 = CARTESIAN_POINT ( 'NONE',  ( 4.771025910096229339, -3543.400907226851814, 2259.826090471561656 ) ) ;
#1329 = EDGE_CURVE ( 'NONE', #2593, #18880, #9040, .T. ) ;
#1330 = AXIS2_PLACEMENT_3D ( 'NONE', #5129, #4880, #7115 ) ;
#1331 = CARTESIAN_POINT ( 'NONE',  ( 12.69999999999999929, -3639.502500000000055, 2290.622800000000097 ) ) ;
#1332 = VECTOR ( 'NONE', #11913, 1000.000000000000000 ) ;
#1333 = DIRECTION ( 'NONE',  ( -1.000000000000000000, 0.000000000000000000, 0.000000000000000000 ) ) ;
#1334 = EDGE_CURVE ( 'NONE', #928, #5746, #19520, .T. ) ;
#1335 = ORIENTED_EDGE ( 'NONE', *, *, #23003, .T. ) ;
#1336 = CIRCLE ( 'NONE', #593, 0.7619999999999987894 ) ;
#1337 = DIRECTION ( 'NONE',  ( 0.000000000000000000, 0.000000000000000000, -1.000000000000000000 ) ) ;
#1338 = DIRECTION ( 'NONE',  ( 0.000000000000000000, 1.000000000000000000, 0.000000000000000000 ) ) ;
#1339 = CARTESIAN_POINT ( 'NONE',  ( 3.048000000000000043, -3544.061999999999898, 2229.612000000000080 ) ) ;
#1340 = FACE_OUTER_BOUND ( 'NONE', #585, .T. ) ;
#1341 = CARTESIAN_POINT ( 'NONE',  ( 41.70680000000000121, -3594.099999999999909, 2239.009999999999764 ) ) ;
#1342 = TOROIDAL_SURFACE ( 'NONE', #7346, 4.114799999999999791, 1.270000000000000018 ) ;
#1343 = EDGE_LOOP ( 'NONE', ( #9952, #15116, #508, #11219 ) ) ;
#1344 = APPROVAL_STATUS ( 'not_yet_approved' ) ;
#1345 = ORIENTED_EDGE ( 'NONE', *, *, #16835, .F. ) ;
#1346 = EDGE_CURVE ( 'NONE', #10418, #1443, #22133, .T. ) ;
#1347 = DIRECTION ( 'NONE',  ( 1.000000000000000000, 0.000000000000000000, 0.000000000000000000 ) ) ;
#1348 = CARTESIAN_POINT ( 'NONE',  ( 10.56087945680325113, -3581.370517028351969, 2248.730192196002918 ) ) ;
#1349 = CARTESIAN_POINT ( 'NONE',  ( 98.75520000000000209, -3670.300000000000182, 2259.837999999999738 ) ) ;
#1350 = EDGE_CURVE ( 'NONE', #6875, #3774, #2663, .T. ) ;
#1351 = ORIENTED_EDGE ( 'NONE', *, *, #1766, .T. ) ;
#1352 = DIRECTION ( 'NONE',  ( 1.000000000000000000, 0.000000000000000000, 0.000000000000000000 ) ) ;
#1353 = EDGE_CURVE ( 'NONE', #20927, #5223, #20628, .T. ) ;
#1354 = VECTOR ( 'NONE', #5449, 1000.000000000000000 ) ;
#1355 = CARTESIAN_POINT ( 'NONE',  ( 12.69999999999999929, -3653.027999999999793, 2268.705139999999574 ) ) ;
#1356 = CARTESIAN_POINT ( 'NONE',  ( 145.2869493186738907, -3660.716514101495250, 2244.602361446073246 ) ) ;
#1357 = CARTESIAN_POINT ( 'NONE',  ( 131.8733694595999850, -3694.556024844999683, 2260.595783923999988 ) ) ;
#1358 = VECTOR ( 'NONE', #19375, 1000.000000000000000 ) ;
#1359 = DIRECTION ( 'NONE',  ( 0.000000000000000000, -1.000000000000000000, 0.000000000000000000 ) ) ;
#1360 = CARTESIAN_POINT ( 'NONE',  ( 147.4837675257009550, -3543.632335307654103, 2260.189864799524003 ) ) ;
#1361 = AXIS2_PLACEMENT_3D ( 'NONE', #1007, #1119, #19060 ) ;
#1362 = ORIENTED_EDGE ( 'NONE', *, *, #10523, .F. ) ;
#1363 = DIRECTION ( 'NONE',  ( -0.000000000000000000, 0.8660254037825932949, 0.5000000000031962211 ) ) ;
#1364 = EDGE_CURVE ( 'NONE', #12078, #18476, #5648, .T. ) ;
#1365 = FACE_BOUND ( 'NONE', #4862, .T. ) ;
#1366 = EDGE_CURVE ( 'NONE', #17007, #3180, #17690, .T. ) ;
#1367 = LINE ( 'NONE', #6541, #15671 ) ;
#1368 = DIRECTION ( 'NONE',  ( 0.000000000000000000, -1.000000000000000000, 0.000000000000000000 ) ) ;
#1369 = DIRECTION ( 'NONE',  ( 0.000000000000000000, 0.000000000000000000, -1.000000000000000000 ) ) ;
#1370 = ORIENTED_EDGE ( 'NONE', *, *, #16592, .F. ) ;
#1371 = VERTEX_POINT ( 'NONE', #21695 ) ;
#1372 = CIRCLE ( 'NONE', #12234, 5.714999999999999858 ) ;
#1373 = PLANE ( 'NONE',  #11313 ) ;
#1374 = ORIENTED_EDGE ( 'NONE', *, *, #10850, .T. ) ;
#1375 = AXIS2_PLACEMENT_3D ( 'NONE', #6437, #18969, #20843 ) ;
#1376 = CARTESIAN_POINT ( 'NONE',  ( 15.21766708706000060, -3580.829381831999854, 2257.881320499000140 ) ) ;
#1377 = AXIS2_PLACEMENT_3D ( 'NONE', #15369, #15259, #22498 ) ;
#1378 = COORDINATED_UNIVERSAL_TIME_OFFSET ( 0, 0, .AHEAD. ) ;
#1379 = CARTESIAN_POINT ( 'NONE',  ( 3.048000000000000043, -3543.299999999999727, 2229.612000000000080 ) ) ;
#1380 = CIRCLE ( 'NONE', #12246, 5.587999999999926359 ) ;
#1381 = CARTESIAN_POINT ( 'NONE',  ( 140.4431196414874989, -3576.742565540147552, 2257.615983594398131 ) ) ;
#1382 = CARTESIAN_POINT ( 'NONE',  ( 12.42421805959000025, -3662.340875907999816, 2257.594929573999707 ) ) ;
#1383 = AXIS2_PLACEMENT_3D ( 'NONE', #7175, #5419, #6343 ) ;
#1384 = CARTESIAN_POINT ( 'NONE',  ( 139.6999999999999886, -3579.494999999999891, 2272.030000000000200 ) ) ;
#1385 = DIRECTION ( 'NONE',  ( 0.000000000000000000, -1.000000000000000000, 0.000000000000000000 ) ) ;
#1386 = CARTESIAN_POINT ( 'NONE',  ( 12.69999999999999929, -3648.710000000000036, 2257.592639999999847 ) ) ;
#1387 = ORIENTED_EDGE ( 'NONE', *, *, #9099, .T. ) ;
#1388 = DIRECTION ( 'NONE',  ( 0.000000000000000000, 1.000000000000000000, 0.000000000000000000 ) ) ;
#1389 = AXIS2_PLACEMENT_3D ( 'NONE', #7265, #4, #3976 ) ;
#1390 = DIRECTION ( 'NONE',  ( -1.000000000000000000, 0.000000000000000000, 0.000000000000000000 ) ) ;
#1391 = ORIENTED_EDGE ( 'NONE', *, *, #15719, .F. ) ;
#1392 = DIRECTION ( 'NONE',  ( 0.000000000000000000, 1.000000000000000000, 0.000000000000000000 ) ) ;
#1393 = CARTESIAN_POINT ( 'NONE',  ( 10.31040564863712561, -3657.961501593514186, 2249.221529667188406 ) ) ;
#1394 = AXIS2_PLACEMENT_3D ( 'NONE', #18019, #7028, #12289 ) ;
#1395 = AXIS2_PLACEMENT_3D ( 'NONE', #9735, #13373, #16539 ) ;
#1396 = VERTEX_POINT ( 'NONE', #17830 ) ;
#1397 = FACE_OUTER_BOUND ( 'NONE', #9744, .T. ) ;
#1398 = VERTEX_POINT ( 'NONE', #18287 ) ;
#1399 = ADVANCED_FACE ( 'NONE', ( #3879 ), #20061, .T. ) ;
#1400 = CARTESIAN_POINT ( 'NONE',  ( 151.4000000000000057, -3578.860000000000127, 2247.392000000000280 ) ) ;
#1401 = EDGE_CURVE ( 'NONE', #17090, #13554, #12783, .T. ) ;
#1402 = COORDINATED_UNIVERSAL_TIME_OFFSET ( 0, 0, .AHEAD. ) ;
#1403 = EDGE_CURVE ( 'NONE', #16556, #1252, #14309, .T. ) ;
#1404 = DIRECTION ( 'NONE',  ( 0.000000000000000000, 0.000000000000000000, -1.000000000000000000 ) ) ;
#1405 = ORIENTED_EDGE ( 'NONE', *, *, #17358, .F. ) ;
#1406 = CARTESIAN_POINT ( 'NONE',  ( 151.1299999999999955, -3694.430000000000291, 2260.600000000000364 ) ) ;
#1407 = CALENDAR_DATE ( 2026, 26, 10 ) ;
#1408 = CARTESIAN_POINT ( 'NONE',  ( 7.619999999999999218, -3579.494999999999891, 2239.391000000000076 ) ) ;
#1409 = CARTESIAN_POINT ( 'NONE',  ( 12.69999999999999929, -3599.497499999999945, 2296.591799999999694 ) ) ;
#1410 = ADVANCED_FACE ( 'NONE', ( #22 ), #13541, .T. ) ;
#1411 = AXIS2_PLACEMENT_3D ( 'NONE', #10840, #17987, #14487 ) ;
#1412 = CARTESIAN_POINT ( 'NONE',  ( 134.2370284977077688, -3657.825934259354199, 2245.736048003489941 ) ) ;
#1413 = CARTESIAN_POINT ( 'NONE',  ( 50.79999999999999716, -3568.700000000000273, 2239.009999999999764 ) ) ;
#1414 = VERTEX_POINT ( 'NONE', #7284 ) ;
#1415 = DIRECTION ( 'NONE',  ( 0.000000000000000000, 0.000000000000000000, -1.000000000000000000 ) ) ;
#1416 = EDGE_CURVE ( 'NONE', #3958, #10503, #14554, .T. ) ;
#1417 = EDGE_CURVE ( 'NONE', #10346, #15928, #14322, .T. ) ;
#1418 = CARTESIAN_POINT ( 'NONE',  ( 12.97550722921000066, -3576.659101291999832, 2257.594923726999696 ) ) ;
#1419 = ORIENTED_EDGE ( 'NONE', *, *, #20266, .F. ) ;
#1420 = DIRECTION ( 'NONE',  ( 0.000000000000000000, 0.000000000000000000, 1.000000000000000000 ) ) ;
#1421 = SHAPE_REPRESENTATION ( 'Magnet Chuck Plate', ( #5611 ), #15735 ) ;
#1422 = CIRCLE ( 'NONE', #8122, 0.7619999999999987894 ) ;
#1423 = DIRECTION ( 'NONE',  ( 1.000000000000000000, 0.000000000000000000, 0.000000000000000000 ) ) ;
#1424 = EDGE_LOOP ( 'NONE', ( #18539, #22099, #12919, #9036 ) ) ;
#1425 = EDGE_LOOP ( 'NONE', ( #2306, #2869, #6704, #11786, #21167, #11479 ) ) ;
#1426 = CARTESIAN_POINT ( 'NONE',  ( 61.26424768829000556, -3544.061999999999898, 2279.065800000000309 ) ) ;
#1427 = ORIENTED_EDGE ( 'NONE', *, *, #3952, .T. ) ;
#1428 = DIRECTION ( 'NONE',  ( 0.000000000000000000, 0.000000000000000000, 1.000000000000000000 ) ) ;
#1429 = CARTESIAN_POINT ( 'NONE',  ( 134.3871257472000025, -3657.399152860999493, 2246.630000000000109 ) ) ;
#1430 =( NAMED_UNIT ( * ) PLANE_ANGLE_UNIT ( ) SI_UNIT ( $, .RADIAN. ) );
#1431 = CARTESIAN_POINT ( 'NONE',  ( 12.69999245750621775, -3642.347301254329977, 2279.817638608992638 ) ) ;
#1432 = CARTESIAN_POINT ( 'NONE',  ( 47.95519999999999783, -3568.700000000000273, 2239.771999999999935 ) ) ;
#1433 = APPLICATION_PROTOCOL_DEFINITION ( 'international standard', 'automotive_design', 2000, #8873 ) ;
#1434 = DIRECTION ( 'NONE',  ( 1.000000000000000000, 0.000000000000000000, 0.000000000000000000 ) ) ;
#1435 = FACE_OUTER_BOUND ( 'NONE', #2011, .T. ) ;
#1436 = CARTESIAN_POINT ( 'NONE',  ( 41.70680000000000121, -3644.899999999999636, 2239.771999999999935 ) ) ;
#1437 = CARTESIAN_POINT ( 'NONE',  ( 141.5035269015962172, -3657.304818365388655, 2247.157352627789805 ) ) ;
#1438 = VERTEX_POINT ( 'NONE', #13237 ) ;
#1439 = CIRCLE ( 'NONE', #4438, 0.7619999999999294005 ) ;
#1440 = CARTESIAN_POINT ( 'NONE',  ( 15.41268679713999923, -3641.068670452857532, 2296.591799999999694 ) ) ;
#1441 = ORIENTED_EDGE ( 'NONE', *, *, #10538, .T. ) ;
#1442 = ORIENTED_EDGE ( 'NONE', *, *, #6454, .F. ) ;
#1443 = VERTEX_POINT ( 'NONE', #14902 ) ;
#1444 = CARTESIAN_POINT ( 'NONE',  ( 55.57575231171000496, -3544.061999999999898, 2275.001800000000003 ) ) ;
#1445 = ORIENTED_EDGE ( 'NONE', *, *, #1366, .F. ) ;
#1446 = VERTEX_POINT ( 'NONE', #2577 ) ;
#1447 = DIRECTION ( 'NONE',  ( 1.000000000000000000, 0.000000000000000000, 0.000000000000000000 ) ) ;
#1448 = COORDINATED_UNIVERSAL_TIME_OFFSET ( 0, 0, .AHEAD. ) ;
#1449 = FACE_OUTER_BOUND ( 'NONE', #20289, .T. ) ;
#1450 = DIRECTION ( 'NONE',  ( 1.000000000000000000, 0.000000000000000000, 0.000000000000000000 ) ) ;
#1451 = VERTEX_POINT ( 'NONE', #4450 ) ;
#1452 = DIRECTION ( 'NONE',  ( 0.000000000000000000, 0.000000000000000000, -1.000000000000000000 ) ) ;
#1453 = CARTESIAN_POINT ( 'NONE',  ( 117.1447999999989946, -3594.099999999999909, 2239.771999999999935 ) ) ;
#1454 = DIRECTION ( 'NONE',  ( 0.000000000000000000, -1.000000000000000000, 0.000000000000000000 ) ) ;
#1455 = TOROIDAL_SURFACE ( 'NONE', #2594, 3.606799999998999695, 0.7620000000000000107 ) ;
#1456 = CARTESIAN_POINT ( 'NONE',  ( 12.69999999997359375, -3596.805099999839967, 2296.433984632673855 ) ) ;
#1457 = EDGE_LOOP ( 'NONE', ( #21375, #6328, #13763, #10041 ) ) ;
#1458 = COORDINATED_UNIVERSAL_TIME_OFFSET ( 0, 0, .AHEAD. ) ;
#1459 = APPLIED_PERSON_AND_ORGANIZATION_ASSIGNMENT ( #5867, #14880, ( #15652 ) ) ;
#1460 = ORIENTED_EDGE ( 'NONE', *, *, #22126, .T. ) ;
#1461 = CARTESIAN_POINT ( 'NONE',  ( 1.270000000000000018, -3694.430000000000291, 2260.600000000000364 ) ) ;
#1462 = CARTESIAN_POINT ( 'NONE',  ( 10.04341343045742541, -3580.512822074882479, 2249.707644168996922 ) ) ;
#1463 = EDGE_CURVE ( 'NONE', #4904, #18111, #16635, .T. ) ;
#1464 = DIRECTION ( 'NONE',  ( 0.000000000000000000, 0.000000000000000000, 1.000000000000000000 ) ) ;
#1465 = ORIENTED_EDGE ( 'NONE', *, *, #10304, .F. ) ;
#1466 = DIRECTION ( 'NONE',  ( 1.000000000000000000, 0.000000000000000000, 0.000000000000000000 ) ) ;
#1467 = AXIS2_PLACEMENT_3D ( 'NONE', #19170, #6756, #21048 ) ;
#1468 = ADVANCED_FACE ( 'NONE', ( #18515 ), #8312, .T. ) ;
#1469 = FACE_OUTER_BOUND ( 'NONE', #5404, .T. ) ;
#1470 = DIRECTION ( 'NONE',  ( -1.000000000000000000, 0.000000000000000000, 0.000000000000000000 ) ) ;
#1471 = DIRECTION ( 'NONE',  ( 0.000000000000000000, 0.000000000000000000, -1.000000000000000000 ) ) ;
#1472 = CARTESIAN_POINT ( 'NONE',  ( 10.56659506800342641, -3661.386912547712200, 2249.948988271942653 ) ) ;
#1473 = CARTESIAN_POINT ( 'NONE',  ( 147.4427523029042106, -3543.741058431988222, 2260.292570800639169 ) ) ;
#1474 = ORIENTED_EDGE ( 'NONE', *, *, #13164, .F. ) ;
#1475 = DIRECTION ( 'NONE',  ( 1.000000000000000000, 0.000000000000000000, 0.000000000000000000 ) ) ;
#1476 = LINE ( 'NONE', #12271, #6217 ) ;
#1477 = CARTESIAN_POINT ( 'NONE',  ( 73.35520000000001062, -3670.300000000000182, 2261.869999999999891 ) ) ;
#1478 = CARTESIAN_POINT ( 'NONE',  ( 25.39999999999999858, -3670.300000000000182, 2261.869999999999891 ) ) ;
#1479 = ORIENTED_EDGE ( 'NONE', *, *, #17226, .F. ) ;
#1480 = ORIENTED_EDGE ( 'NONE', *, *, #7960, .T. ) ;
#1481 = VECTOR ( 'NONE', #692, 1000.000000000000000 ) ;
#1482 = CARTESIAN_POINT ( 'NONE',  ( 6.985000000000999520, -3599.497499999999945, 2288.971800000000258 ) ) ;
#1483 = APPLIED_APPROVAL_ASSIGNMENT ( #16363, ( #20503 ) ) ;
#1484 = VERTEX_POINT ( 'NONE', #13128 ) ;
#1485 =( GEOMETRIC_REPRESENTATION_CONTEXT ( 3 ) GLOBAL_UNCERTAINTY_ASSIGNED_CONTEXT ( ( #20035 ) ) GLOBAL_UNIT_ASSIGNED_CONTEXT ( ( #19015, #6484, #13749 ) ) REPRESENTATION_CONTEXT ( 'NONE', 'WORKASPACE' ) );
#1486 = CARTESIAN_POINT ( 'NONE',  ( 9.847598318245756488, -3543.397347667041686, 2254.991658123818070 ) ) ;
#1487 = DIRECTION ( 'NONE',  ( 0.000000000000000000, -1.000000000000000000, 0.000000000000000000 ) ) ;
#1488 = ADVANCED_FACE ( 'NONE', ( #13471 ), #6444, .T. ) ;
#1489 = CARTESIAN_POINT ( 'NONE',  ( 9.970475488813999476, -3658.687501247999990, 2257.932973791000222 ) ) ;
#1490 = CARTESIAN_POINT ( 'NONE',  ( 11.12257588577000078, -3661.878010978000020, 2257.704312134999782 ) ) ;
#1491 = EDGE_CURVE ( 'NONE', #21023, #8893, #19537, .T. ) ;
#1492 = FACE_OUTER_BOUND ( 'NONE', #22547, .T. ) ;
#1493 = EDGE_CURVE ( 'NONE', #15348, #5042, #16896, .T. ) ;
#1494 = CARTESIAN_POINT ( 'NONE',  ( 136.6529205195000145, -3695.699999999999818, 2254.503999999999905 ) ) ;
#1495 = CARTESIAN_POINT ( 'NONE',  ( 12.69999999999999929, -3599.497499999999945, 2290.622800000000097 ) ) ;
#1496 = ORIENTED_EDGE ( 'NONE', *, *, #16738, .F. ) ;
#1497 = VECTOR ( 'NONE', #13193, 1000.000000000000114 ) ;
#1498 = PLANE ( 'NONE',  #11810 ) ;
#1499 = DIRECTION ( 'NONE',  ( 0.000000000000000000, 0.000000000000000000, 1.000000000000000000 ) ) ;
#1500 = EDGE_LOOP ( 'NONE', ( #4367, #7166, #13734, #10540 ) ) ;
#1501 = LOCAL_TIME ( 17, 37, 43.00000000000000000, #6672 ) ;
#1502 = CARTESIAN_POINT ( 'NONE',  ( 20.32000000000000028, -3670.300000000000182, 2286.368300000000090 ) ) ;
#1503 = LOCAL_TIME ( 17, 37, 43.00000000000000000, #12185 ) ;
#1504 = CARTESIAN_POINT ( 'NONE',  ( 139.7000000000063835, -3576.802599999938593, 2239.391000000000076 ) ) ;
#1505 = AXIS2_PLACEMENT_3D ( 'NONE', #8930, #373, #10574 ) ;
#1506 = ORIENTED_EDGE ( 'NONE', *, *, #17845, .T. ) ;
#1507 = CIRCLE ( 'NONE', #14628, 5.715000000001058567 ) ;
#1508 = CARTESIAN_POINT ( 'NONE',  ( 134.1443423388099063, -3580.833646875505110, 2245.342901023084778 ) ) ;
#1509 = EDGE_CURVE ( 'NONE', #7148, #4633, #7924, .T. ) ;
#1510 = VERTEX_POINT ( 'NONE', #5994 ) ;
#1511 = EDGE_LOOP ( 'NONE', ( #17122, #8906 ) ) ;
#1512 = PRODUCT_DEFINITION_SHAPE ( 'NONE', 'NONE',  #5365 ) ;
#1513 = DIRECTION ( 'NONE',  ( 0.000000000000000000, 0.000000000000000000, 1.000000000000000000 ) ) ;
#1514 = APPROVAL_STATUS ( 'not_yet_approved' ) ;
#1515 = CARTESIAN_POINT ( 'NONE',  ( 7.619999999999999218, -3599.497499999999945, 2290.241799999999785 ) ) ;
#1516 = EDGE_LOOP ( 'NONE', ( #13022, #20332, #9666, #3962 ) ) ;
#1517 = CARTESIAN_POINT ( 'NONE',  ( 131.7616391464439971, -3695.609040584405193, 2259.802577514632958 ) ) ;
#1518 = PERSON_AND_ORGANIZATION ( #5446, #1895 ) ;
#1519 = DIRECTION ( 'NONE',  ( -0.7071067811860285435, 0.000000000000000000, -0.7071067811870666020 ) ) ;
#1520 = APPROVAL_PERSON_ORGANIZATION ( #3598, #20631, #21071 ) ;
#1521 = CARTESIAN_POINT ( 'NONE',  ( 15.45570990063155392, -3580.206700319643460, 2249.899904268654154 ) ) ;
#1522 = LOCAL_TIME ( 17, 37, 43.00000000000000000, #20207 ) ;
#1523 = CARTESIAN_POINT ( 'NONE',  ( 50.79999999999999716, -3619.500000000000000, 2239.771999999999935 ) ) ;
#1524 = ADVANCED_FACE ( 'NONE', ( #7860 ), #18632, .F. ) ;
#1525 = CARTESIAN_POINT ( 'NONE',  ( 151.1299999999999955, -3694.430000000000291, 2240.279999999999745 ) ) ;
#1526 = CARTESIAN_POINT ( 'NONE',  ( 12.70000000000000107, -3590.289999999999964, 2279.817639999999756 ) ) ;
#1527 = ORIENTED_EDGE ( 'NONE', *, *, #18311, .F. ) ;
#1528 = CARTESIAN_POINT ( 'NONE',  ( 28.24479999999899604, -3619.500000000000000, 2261.869999999999891 ) ) ;
#1529 = EDGE_CURVE ( 'NONE', #4464, #10440, #9436, .T. ) ;
#1530 = CIRCLE ( 'NONE', #15007, 0.7619999999999294005 ) ;
#1531 = EDGE_CURVE ( 'NONE', #14575, #12638, #18031, .T. ) ;
#1532 = CARTESIAN_POINT ( 'NONE',  ( -12.31899999999987827, -3576.167599999831964, 2247.391999999993914 ) ) ;
#1533 = ORIENTED_EDGE ( 'NONE', *, *, #7543, .T. ) ;
#1534 = LINE ( 'NONE', #20757, #22196 ) ;
#1535 = CARTESIAN_POINT ( 'NONE',  ( 12.70000000002425899, -3662.197400000083690, 2239.391000000000076 ) ) ;
#1536 = ORIENTED_EDGE ( 'NONE', *, *, #19257, .F. ) ;
#1537 = ORIENTED_EDGE ( 'NONE', *, *, #16396, .F. ) ;
#1538 = CARTESIAN_POINT ( 'NONE',  ( 127.0000000000000000, -3619.500000000000000, 2261.869999999999891 ) ) ;
#1539 = CARTESIAN_POINT ( 'NONE',  ( 12.69999999999999929, -3659.504999999999654, 2245.359999999999673 ) ) ;
#1540 = EDGE_CURVE ( 'NONE', #13123, #14851, #5320, .T. ) ;
#1541 = VERTEX_POINT ( 'NONE', #597 ) ;
#1542 = DIRECTION ( 'NONE',  ( -1.000000000000000000, 0.000000000000000000, 0.000000000000000000 ) ) ;
#1543 = CARTESIAN_POINT ( 'NONE',  ( -12.70000000000011831, -3660.140000000000327, 2242.311999999999898 ) ) ;
#1544 = CARTESIAN_POINT ( 'NONE',  ( 15.54479999999999862, -3599.497499999999945, 2279.447335734999797 ) ) ;
#1546 = CARTESIAN_POINT ( 'NONE',  ( 136.9109231113999954, -3578.930102841999997, 2250.236803302000226 ) ) ;
#1545 = AXIS2_PLACEMENT_3D ( 'NONE', #16930, #6293, #20459 ) ;
#1547 = ADVANCED_FACE ( 'NONE', ( #2687, #15240 ), #20170, .F. ) ;
#1548 = SECURITY_CLASSIFICATION_LEVEL ( 'unclassified' ) ;
#1549 = AXIS2_PLACEMENT_3D ( 'NONE', #16667, #9524, #18765 ) ;
#1550 = ADVANCED_FACE ( 'NONE', ( #4225 ), #13361, .T. ) ;
#1551 = CARTESIAN_POINT ( 'NONE',  ( 151.6380000000000052, -3544.061999999999898, 2279.827800000000025 ) ) ;
#1552 = CARTESIAN_POINT ( 'NONE',  ( 9.851292762693375948, -3695.598810868125383, 2255.000759462867791 ) ) ;
#1553 = DIRECTION ( 'NONE',  ( 0.000000000000000000, -1.000000000000000000, 0.000000000000000000 ) ) ;
#1554 = CARTESIAN_POINT ( 'NONE',  ( 0.000000000000000000, -3694.430000000000291, 2259.329999999999927 ) ) ;
#1555 = ORIENTED_EDGE ( 'NONE', *, *, #2631, .F. ) ;
#1556 = CARTESIAN_POINT ( 'NONE',  ( 142.0316867971999955, -3660.851200000000063, 2242.820000000000164 ) ) ;
#1557 = EDGE_CURVE ( 'NONE', #8915, #6279, #4988, .T. ) ;
#1558 = EDGE_LOOP ( 'NONE', ( #1774, #9639 ) ) ;
#1559 = ORIENTED_EDGE ( 'NONE', *, *, #3188, .F. ) ;
#1560 = ORIENTED_EDGE ( 'NONE', *, *, #14314, .F. ) ;
#1561 = CIRCLE ( 'NONE', #9435, 2.844800000000091700 ) ;
#1562 = AXIS2_PLACEMENT_3D ( 'NONE', #810, #22367, #22246 ) ;
#1563 = DIRECTION ( 'NONE',  ( 0.000000000000000000, 0.000000000000000000, 1.000000000000000000 ) ) ;
#1564 = ORIENTED_EDGE ( 'NONE', *, *, #1037, .T. ) ;
#1565 = ORIENTED_EDGE ( 'NONE', *, *, #18959, .T. ) ;
#1566 = LINE ( 'NONE', #21266, #17250 ) ;
#1567 = ITEM_DEFINED_TRANSFORMATION ( 'NONE', 'NONE', #13106,  #5611 ) ;
#1568 = CARTESIAN_POINT ( 'NONE',  ( 76.20000000000000284, -3670.300000000000182, 2261.869999999999891 ) ) ;
#1569 = B_SPLINE_CURVE_WITH_KNOTS ( 'NONE', 3,
 ( #22774, #19748, #7546, #17977 ),
 .UNSPECIFIED., .F., .F.,
 ( 4, 4 ),
 ( 0.000000000000000000, 3.168591426078754222E-06 ),
 .UNSPECIFIED. ) ;
#1570 = CARTESIAN_POINT ( 'NONE',  ( 15.03168679717000167, -3660.851200000000063, 2242.820000000000164 ) ) ;
#1571 = ORIENTED_EDGE ( 'NONE', *, *, #2628, .F. ) ;
#1572 = CARTESIAN_POINT ( 'NONE',  ( 25.39999999999999858, -3670.300000000000182, 2239.009999999999764 ) ) ;
#1573 = FACE_BOUND ( 'NONE', #14091, .T. ) ;
#1574 = CARTESIAN_POINT ( 'NONE',  ( 11.65131536725999872, -3544.061999999999898, 2286.653115367000282 ) ) ;
#1575 = CYLINDRICAL_SURFACE ( 'NONE', #4354, 0.7620000000000001217 ) ;
#1576 = AXIS2_PLACEMENT_3D ( 'NONE', #17280, #8391, #4865 ) ;
#1577 = ORIENTED_EDGE ( 'NONE', *, *, #14313, .T. ) ;
#1578 = EDGE_CURVE ( 'NONE', #22298, #2067, #1046, .T. ) ;
#1579 = DATE_AND_TIME ( #5336, #13495 ) ;
#1580 = ORIENTED_EDGE ( 'NONE', *, *, #11641, .T. ) ;
#1581 = DIRECTION ( 'NONE',  ( 1.000000000000000000, 0.000000000000000000, 0.000000000000000000 ) ) ;
#1582 = CIRCLE ( 'NONE', #17670, 3.175000000000149925 ) ;
#1583 = CARTESIAN_POINT ( 'NONE',  ( 10.57556485081456898, -3581.387054496447035, 2248.698531430067760 ) ) ;
#1584 = DIRECTION ( 'NONE',  ( 0.000000000000000000, 1.000000000000000000, 0.000000000000000000 ) ) ;
#1585 = ORIENTED_EDGE ( 'NONE', *, *, #14722, .T. ) ;
#1586 = CARTESIAN_POINT ( 'NONE',  ( 76.20000000000000284, -3670.300000000000182, 2239.771999999999935 ) ) ;
#1587 = DIRECTION ( 'NONE',  ( 0.000000000000000000, -1.000000000000000000, 0.000000000000000000 ) ) ;
#1588 = FACE_BOUND ( 'NONE', #11357, .T. ) ;
#1589 = CARTESIAN_POINT ( 'NONE',  ( 152.4000000000000057, -3694.938000000000102, 2295.829799999999977 ) ) ;
#1590 = AXIS2_PLACEMENT_3D ( 'NONE', #15714, #9850, #22843 ) ;
#1591 = CARTESIAN_POINT ( 'NONE',  ( 11.62623776245822249, -3662.139701344950481, 2249.415671503285921 ) ) ;
#1592 = DIRECTION ( 'NONE',  ( 1.000000000000000000, 0.000000000000000000, 0.000000000000000000 ) ) ;
#1593 = VERTEX_POINT ( 'NONE', #21921 ) ;
#1594 = CARTESIAN_POINT ( 'NONE',  ( 35.56000000000000227, -3695.699999999999818, 2251.506800000000112 ) ) ;
#1595 = DIRECTION ( 'NONE',  ( 0.000000000000000000, 0.000000000000000000, 1.000000000000000000 ) ) ;
#1596 = CIRCLE ( 'NONE', #18805, 0.7619999999999996776 ) ;
#1597 = CARTESIAN_POINT ( 'NONE',  ( 134.2390000000000043, -3579.494999999999891, 2244.978999999999814 ) ) ;
#1598 = CARTESIAN_POINT ( 'NONE',  ( 14.52771269207012850, -3657.324844698252491, 2247.803865992611463 ) ) ;
#1599 = CARTESIAN_POINT ( 'NONE',  ( 10.36831320289401859, -3640.848700000111421, 2296.210799999999836 ) ) ;
#1600 = ORIENTED_EDGE ( 'NONE', *, *, #16524, .F. ) ;
#1601 = CARTESIAN_POINT ( 'NONE',  ( 147.3199999999999932, -3544.570000000000164, 2260.600000000000364 ) ) ;
#1602 = EDGE_LOOP ( 'NONE', ( #22191, #17975, #17577, #13431 ) ) ;
#1603 = DIRECTION ( 'NONE',  ( 1.000000000000000000, 5.432398939370942693E-28, -2.324635735433000053E-14 ) ) ;
#1604 = CARTESIAN_POINT ( 'NONE',  ( -5.588000000000000078, -3694.938000000000102, 2229.612000000000080 ) ) ;
#1605 = CIRCLE ( 'NONE', #15833, 0.7619999999999987894 ) ;
#1606 = DIRECTION ( 'NONE',  ( -1.000000000000000000, 0.000000000000000000, -1.295098308109999907E-13 ) ) ;
#1607 = CARTESIAN_POINT ( 'NONE',  ( 9.855200508358999301, -3659.413078923999819, 2257.962940201000038 ) ) ;
#1608 = DIRECTION ( 'NONE',  ( 0.000000000000000000, 1.000000000000000000, 0.000000000000000000 ) ) ;
#1609 = VECTOR ( 'NONE', #2505, 1000.000000000000000 ) ;
#1610 = DIRECTION ( 'NONE',  ( 0.7249994335945011414, 0.000000000000000000, -0.6887494619146010688 ) ) ;
#1611 = CARTESIAN_POINT ( 'NONE',  ( 12.69999999999999929, -3649.471999999999753, 2262.355140000000119 ) ) ;
#1612 = AXIS2_PLACEMENT_3D ( 'NONE', #19935, #10675, #3875 ) ;
#1613 = DIRECTION ( 'NONE',  ( 1.000000000000000000, 5.432398939370942693E-28, -2.324635735433000053E-14 ) ) ;
#1614 = ORIENTED_EDGE ( 'NONE', *, *, #9995, .F. ) ;
#1615 = DIRECTION ( 'NONE',  ( -2.318894227180156550E-14, -1.000000000000000000, 0.000000000000000000 ) ) ;
#1616 = APPROVAL ( #1344, 'UNSPECIFIED' ) ;
#1617 = DIRECTION ( 'NONE',  ( -1.000000000000000000, -0.000000000000000000, -0.000000000000000000 ) ) ;
#1618 = ORIENTED_EDGE ( 'NONE', *, *, #434, .T. ) ;
#1619 = DIRECTION ( 'NONE',  ( 0.000000000000000000, 0.000000000000000000, -1.000000000000000000 ) ) ;
#1620 = CIRCLE ( 'NONE', #11354, 2.844799999999009010 ) ;
#1621 = EDGE_CURVE ( 'NONE', #10003, #16281, #13024, .T. ) ;
#1622 = CIRCLE ( 'NONE', #16579, 0.7619999999999294005 ) ;
#1623 = ORIENTED_EDGE ( 'NONE', *, *, #19115, .T. ) ;
#1624 = DIRECTION ( 'NONE',  ( 0.000000000000000000, 0.000000000000000000, 1.000000000000000000 ) ) ;
#1625 = EDGE_CURVE ( 'NONE', #7999, #4345, #19946, .T. ) ;
#1626 = ORIENTED_EDGE ( 'NONE', *, *, #3283, .F. ) ;
#1627 = ORIENTED_EDGE ( 'NONE', *, *, #333, .F. ) ;
#1628 = EDGE_CURVE ( 'NONE', #19068, #19181, #15812, .T. ) ;
#1629 = VECTOR ( 'NONE', #3520, 999.9999999999998863 ) ;
#1630 = LINE ( 'NONE', #15473, #15052 ) ;
#1631 = ORIENTED_EDGE ( 'NONE', *, *, #8221, .F. ) ;
#1632 = CARTESIAN_POINT ( 'NONE',  ( 9.209369265603214672, -3695.699999999999818, 2282.113800000000083 ) ) ;
#1633 = PERSON_AND_ORGANIZATION ( #5446, #1895 ) ;
#1634 = DIRECTION ( 'NONE',  ( 0.000000000000000000, 0.000000000000000000, -1.000000000000000000 ) ) ;
#1635 = EDGE_CURVE ( 'NONE', #20696, #7575, #5699, .T. ) ;
#1636 = DIRECTION ( 'NONE',  ( 0.000000000000000000, 1.000000000000000000, 0.000000000000000000 ) ) ;
#1637 = VECTOR ( 'NONE', #5851, 1000.000000000000114 ) ;
#1638 = DIRECTION ( 'NONE',  ( 0.000000000000000000, -1.000000000000000000, 0.000000000000000000 ) ) ;
#1639 = DIRECTION ( 'NONE',  ( -0.5000000000031612490, -0.8660254037826135010, 0.000000000000000000 ) ) ;
#1640 = EDGE_CURVE ( 'NONE', #17185, #6183, #20730, .T. ) ;
#1641 = CARTESIAN_POINT ( 'NONE',  ( 3.810000000000000053, -3544.061999999999898, 2229.612000000000080 ) ) ;
#1642 = EDGE_LOOP ( 'NONE', ( #22112, #11847, #7529, #9622 ) ) ;
#1643 = DIRECTION ( 'NONE',  ( 4.703417536272999698E-14, 1.000000000000000000, 2.474126484833999786E-12 ) ) ;
#1644 = ADVANCED_FACE ( 'NONE', ( #6570 ), #3152, .F. ) ;
#1645 = CARTESIAN_POINT ( 'NONE',  ( 15.54479972196000048, -3579.494985918000111, 2257.962943248000101 ) ) ;
#1646 = ORIENTED_EDGE ( 'NONE', *, *, #21568, .F. ) ;
#1647 = CARTESIAN_POINT ( 'NONE',  ( 5.032733771186362226, -3695.066554911154071, 2260.481515824936196 ) ) ;
#1648 = CARTESIAN_POINT ( 'NONE',  ( 12.69999999999999929, -3590.289999999999964, 2268.705139999999574 ) ) ;
#1649 = CARTESIAN_POINT ( 'NONE',  ( 0.000000000000000000, -3544.570000000000164, 2259.329999999999927 ) ) ;
#1650 = VERTEX_POINT ( 'NONE', #17447 ) ;
#1651 = DIRECTION ( 'NONE',  ( 0.5000000000040877302, 0.8660254037820785955, 0.000000000000000000 ) ) ;
#1652 = LINE ( 'NONE', #5299, #6943 ) ;
#1653 = CIRCLE ( 'NONE', #15143, 2.844800000000091700 ) ;
#1654 = ORIENTED_EDGE ( 'NONE', *, *, #17458, .T. ) ;
#1656 = EDGE_CURVE ( 'NONE', #9562, #2027, #3807, .T. ) ;
#1655 = TOROIDAL_SURFACE ( 'NONE', #6961, 5.080000000000000071, 0.3810000000000000053 ) ;
#1657 = CARTESIAN_POINT ( 'NONE',  ( 91.74479999999999791, -3594.099999999999909, 2261.869999999999891 ) ) ;
#1658 = FACE_OUTER_BOUND ( 'NONE', #3586, .T. ) ;
#1659 =( NAMED_UNIT ( * ) PLANE_ANGLE_UNIT ( ) SI_UNIT ( $, .RADIAN. ) );
#1660 = AXIS2_PLACEMENT_3D ( 'NONE', #20002, #313, #3934 ) ;
#1661 = DIRECTION ( 'NONE',  ( 0.000000000000000000, 0.000000000000000000, -1.000000000000000000 ) ) ;
#1662 = PERSON_AND_ORGANIZATION_ROLE ( 'creator' ) ;
#1663 = EDGE_CURVE ( 'NONE', #18199, #7611, #8000, .T. ) ;
#1664 = ADVANCED_FACE ( 'NONE', ( #1397 ), #10921, .T. ) ;
#1665 = CARTESIAN_POINT ( 'NONE',  ( 137.3683132029851208, -3660.851200000049630, 2239.391000000000076 ) ) ;
#1666 = DIRECTION ( 'NONE',  ( 0.000000000000000000, -1.000000000000000000, 0.000000000000000000 ) ) ;
#1667 = CARTESIAN_POINT ( 'NONE',  ( 10.36831320284000135, -3635.463900000000194, 2292.781800000000203 ) ) ;
#1668 = CARTESIAN_POINT ( 'NONE',  ( 137.1312382075398375, -3658.282264947529711, 2249.547148403314168 ) ) ;
#1669 = AXIS2_PLACEMENT_3D ( 'NONE', #19032, #13877, #15867 ) ;
#1670 = ORIENTED_EDGE ( 'NONE', *, *, #1640, .T. ) ;
#1671 = CIRCLE ( 'NONE', #20758, 4.114799999999974034 ) ;
#1672 = CARTESIAN_POINT ( 'NONE',  ( 137.0047131064691541, -3660.427569099905668, 2250.225733703707192 ) ) ;
#1673 = AXIS2_PLACEMENT_3D ( 'NONE', #5293, #20908, #17823 ) ;
#1674 = APPLICATION_CONTEXT ( 'configuration controlled 3d designs of mechanical parts and assemblies' ) ;
#1675 = EDGE_LOOP ( 'NONE', ( #17011, #16139 ) ) ;
#1676 = AXIS2_PLACEMENT_3D ( 'NONE', #11507, #20525, #17009 ) ;
#1677 = VERTEX_POINT ( 'NONE', #22829 ) ;
#1678 = ORIENTED_EDGE ( 'NONE', *, *, #2220, .F. ) ;
#1679 = EDGE_CURVE ( 'NONE', #15928, #21490, #19108, .T. ) ;
#1680 = CARTESIAN_POINT ( 'NONE',  ( 12.69999999999999929, -3585.210000000000036, 2275.055139999999483 ) ) ;
#1681 = ORIENTED_EDGE ( 'NONE', *, *, #21603, .T. ) ;
#1682 = EDGE_LOOP ( 'NONE', ( #12031, #5258, #388, #6450 ) ) ;
#1683 = DIRECTION ( 'NONE',  ( 0.000000000000000000, 0.000000000000000000, 1.000000000000000000 ) ) ;
#1684 = DATE_AND_TIME ( #8956, #6418 ) ;
#1685 = DIRECTION ( 'NONE',  ( 0.000000000000000000, 0.000000000000000000, -1.000000000000000000 ) ) ;
#1686 = DIRECTION ( 'NONE',  ( 0.000000000000000000, 0.000000000000000000, 1.000000000000000000 ) ) ;
#1687 = EDGE_LOOP ( 'NONE', ( #8535, #1801, #12779, #20172 ) ) ;
#1688 = DIRECTION ( 'NONE',  ( 0.000000000000000000, 0.000000000000000000, -1.000000000000000000 ) ) ;
#1689 = FACE_BOUND ( 'NONE', #7308, .T. ) ;
#1690 = CARTESIAN_POINT ( 'NONE',  ( 20.32000000000000028, -3568.700000000000273, 2289.213099999999940 ) ) ;
#1691 = AXIS2_PLACEMENT_3D ( 'NONE', #4081, #3644, #679 ) ;
#1692 = AXIS2_PLACEMENT_3D ( 'NONE', #3746, #18052, #11019 ) ;
#1693 = CARTESIAN_POINT ( 'NONE',  ( 47.19319999999999737, -3670.300000000000182, 2239.009999999999764 ) ) ;
#1694 = VERTEX_POINT ( 'NONE', #19333 ) ;
#1695 = PERSON_AND_ORGANIZATION ( #5446, #1895 ) ;
#1696 = AXIS2_PLACEMENT_3D ( 'NONE', #22716, #22825, #10413 ) ;
#1697 = EDGE_CURVE ( 'NONE', #13127, #5536, #12054, .T. ) ;
#1698 = ORIENTED_EDGE ( 'NONE', *, *, #13499, .F. ) ;
#1699 = AXIS2_PLACEMENT_3D ( 'NONE', #5913, #4591, #8121 ) ;
#1700 = CARTESIAN_POINT ( 'NONE',  ( 9.855258736895999405, -3579.517414328000086, 2250.159819663000235 ) ) ;
#1701 = EDGE_CURVE ( 'NONE', #13004, #4281, #19168, .T. ) ;
#1702 = CARTESIAN_POINT ( 'NONE',  ( 55.57575231171000496, -3544.061999999999898, 2275.001800000000003 ) ) ;
#1703 = DIRECTION ( 'NONE',  ( 0.000000000000000000, 0.000000000000000000, -1.000000000000000000 ) ) ;
#1704 = ADVANCED_FACE ( 'NONE', ( #3616 ), #15056, .T. ) ;
#1705 = ORIENTED_EDGE ( 'NONE', *, *, #23112, .F. ) ;
#1706 = DIRECTION ( 'NONE',  ( 1.000000000000000000, 0.000000000000000000, 0.000000000000000000 ) ) ;
#1707 = AXIS2_PLACEMENT_3D ( 'NONE', #16017, #14154, #13911 ) ;
#1708 = CARTESIAN_POINT ( 'NONE',  ( 142.5447999999989861, -3579.494999999999891, 2272.030000000000200 ) ) ;
#1709 = FACE_OUTER_BOUND ( 'NONE', #21775, .T. ) ;
#1710 = CARTESIAN_POINT ( 'NONE',  ( 132.0286855373999799, -3694.758336080999925, 2260.557504193999648 ) ) ;
#1711 = AXIS2_PLACEMENT_3D ( 'NONE', #4187, #3961, #11332 ) ;
#1712 = EDGE_CURVE ( 'NONE', #1677, #10545, #1185, .T. ) ;
#1713 = DIRECTION ( 'NONE',  ( -1.000000000000000000, 0.000000000000000000, -2.902585187577999742E-13 ) ) ;
#1714 = PRODUCT_DEFINITION_SHAPE ( 'NONE', 'NONE',  #22959 ) ;
#1715 = VERTEX_POINT ( 'NONE', #23062 ) ;
#1716 =( REPRESENTATION_RELATIONSHIP ('NONE','NONE', #20448, #8615 ) REPRESENTATION_RELATIONSHIP_WITH_TRANSFORMATION ( #10517 )SHAPE_REPRESENTATION_RELATIONSHIP( ) );
#1717 = AXIS2_PLACEMENT_3D ( 'NONE', #22465, #4786, #11930 ) ;
#1718 = ADVANCED_FACE ( 'NONE', ( #21669 ), #232, .T. ) ;
#1719 = CARTESIAN_POINT ( 'NONE',  ( 19.05000000000000071, -3660.140000000000327, 2247.392000000000280 ) ) ;
#1720 = AXIS2_PLACEMENT_3D ( 'NONE', #22933, #19555, #21082 ) ;
#1721 = ORIENTED_EDGE ( 'NONE', *, *, #11917, .F. ) ;
#1722 = PLANE ( 'NONE',  #12133 ) ;
#1723 = VECTOR ( 'NONE', #4700, 1000.000000000000000 ) ;
#1724 = CARTESIAN_POINT ( 'NONE',  ( 55.57575231171000496, -3695.699999999999818, 2275.763800000000174 ) ) ;
#1725 = DIRECTION ( 'NONE',  ( -2.879814920640999944E-14, -1.000000000000000000, -1.559530541638999969E-12 ) ) ;
#1726 = CARTESIAN_POINT ( 'NONE',  ( 15.17971944497489467, -3658.110408443104006, 2249.386264408048191 ) ) ;
#1727 = CARTESIAN_POINT ( 'NONE',  ( 136.8052632656678895, -3695.644174308496986, 2254.886265309746705 ) ) ;
#1728 = EDGE_LOOP ( 'NONE', ( #22366, #22048, #22055, #11818 ) ) ;
#1729 = DIRECTION ( 'NONE',  ( 0.000000000000000000, 0.000000000000000000, -1.000000000000000000 ) ) ;
#1730 = ORIENTED_EDGE ( 'NONE', *, *, #19464, .T. ) ;
#1731 = AXIS2_PLACEMENT_3D ( 'NONE', #15996, #10603, #15649 ) ;
#1732 = CARTESIAN_POINT ( 'NONE',  ( 12.69999999999999929, -3655.060000000000400, 2268.705139999999574 ) ) ;
#1733 = CIRCLE ( 'NONE', #21933, 2.844799999999994444 ) ;
#1734 = DIRECTION ( 'NONE',  ( 0.000000000000000000, -1.000000000000000000, 0.000000000000000000 ) ) ;
#1735 = DATE_AND_TIME ( #12509, #16135 ) ;
#1736 = LINE ( 'NONE', #5020, #1956 ) ;
#1737 = AXIS2_PLACEMENT_3D ( 'NONE', #20723, #11694, #4669 ) ;
#1738 = DIRECTION ( 'NONE',  ( 0.000000000000000000, 0.000000000000000000, -1.000000000000000000 ) ) ;
#1739 = CARTESIAN_POINT ( 'NONE',  ( 139.6999999999999886, -3576.650200000000950, 2257.592639999999847 ) ) ;
#1740 = TOROIDAL_SURFACE ( 'NONE', #17825, 1.905000000000000027, 1.270000000000000018 ) ;
#1741 = CARTESIAN_POINT ( 'NONE',  ( 72.56166137651000270, -3694.430000000000291, 2315.390696186000241 ) ) ;
#1742 = VERTEX_POINT ( 'NONE', #2106 ) ;
#1743 = DIRECTION ( 'NONE',  ( 0.000000000000000000, 0.000000000000000000, 1.000000000000000000 ) ) ;
#1744 = EDGE_LOOP ( 'NONE', ( #17388, #21682, #4617, #3315 ) ) ;
#1745 = CARTESIAN_POINT ( 'NONE',  ( -6.349999999999999645, -3543.299999999999727, 2254.250000000000000 ) ) ;
#1746 = DIRECTION ( 'NONE',  ( 0.000000000000000000, 0.000000000000000000, 1.000000000000000000 ) ) ;
#1747 = ORIENTED_EDGE ( 'NONE', *, *, #9104, .F. ) ;
#1748 = DIRECTION ( 'NONE',  ( -3.627287058276000189E-13, 1.295098308114999897E-13, 1.000000000000000000 ) ) ;
#1749 = VECTOR ( 'NONE', #4374, 1000.000000000000000 ) ;
#1750 = EDGE_LOOP ( 'NONE', ( #12144, #21234 ) ) ;
#1751 = DIRECTION ( 'NONE',  ( 0.000000000000000000, -1.000000000000000000, 0.000000000000000000 ) ) ;
#1752 = CARTESIAN_POINT ( 'NONE',  ( 142.4995878314999800, -3660.024017658000048, 2250.236800000000130 ) ) ;
#1753 = ORIENTED_EDGE ( 'NONE', *, *, #9708, .T. ) ;
#1754 = ORIENTED_EDGE ( 'NONE', *, *, #20889, .F. ) ;
#1755 = ORIENTED_EDGE ( 'NONE', *, *, #21279, .T. ) ;
#1756 = CARTESIAN_POINT ( 'NONE',  ( 137.3720204532196476, -3581.130476171526880, 2249.106963701437962 ) ) ;
#1757 = ORIENTED_EDGE ( 'NONE', *, *, #5135, .T. ) ;
#1758 = PERSON_AND_ORGANIZATION ( #5446, #1895 ) ;
#1759 = PRODUCT_DEFINITION ( 'UNKNOWN', '', #10100, #20731 ) ;
#1760 = DIRECTION ( 'NONE',  ( 0.000000000000000000, 1.000000000000000000, 0.000000000000000000 ) ) ;
#1761 = DIRECTION ( 'NONE',  ( 0.000000000000000000, 1.000000000000000000, 0.000000000000000000 ) ) ;
#1762 = CIRCLE ( 'NONE', #21961, 4.114799999999974034 ) ;
#1763 = DIRECTION ( 'NONE',  ( 0.8660254037841628172, 0.5000000000004778400, -5.443078266502769467E-12 ) ) ;
#1764 = LINE ( 'NONE', #6929, #9474 ) ;
#1765 = VECTOR ( 'NONE', #1189, 1000.000000000000114 ) ;
#1766 = EDGE_CURVE ( 'NONE', #3129, #11209, #9784, .T. ) ;
#1767 = ADVANCED_FACE ( 'NONE', ( #21439 ), #16047, .F. ) ;
#1768 = CARTESIAN_POINT ( 'NONE',  ( 15.03168679716000078, -3578.148799999999937, 2239.391000000000076 ) ) ;
#1769 = ORIENTED_EDGE ( 'NONE', *, *, #7092, .T. ) ;
#1770 = CARTESIAN_POINT ( 'NONE',  ( 64.76999999999999602, -3544.061999999999898, 2289.213099999999940 ) ) ;
#1771 = EDGE_CURVE ( 'NONE', #16761, #3671, #22510, .T. ) ;
#1772 = AXIS2_PLACEMENT_3D ( 'NONE', #7987, #378, #20072 ) ;
#1773 = CARTESIAN_POINT ( 'NONE',  ( 15.42952381853999988, -3578.677498958000342, 2257.932973515999947 ) ) ;
#1774 = ORIENTED_EDGE ( 'NONE', *, *, #4675, .T. ) ;
#1775 = CARTESIAN_POINT ( 'NONE',  ( 4.742867852766174508, -3695.626565543418110, 2259.755970531261028 ) ) ;
#1776 = PLANE ( 'NONE',  #9856 ) ;
#1777 = CARTESIAN_POINT ( 'NONE',  ( 20.12315942192000051, -3544.527728670999750, 2260.413001451000127 ) ) ;
#1778 = EDGE_LOOP ( 'NONE', ( #14987, #13379, #9900, #1833 ) ) ;
#1779 = EDGE_CURVE ( 'NONE', #17500, #17093, #15210, .T. ) ;
#1780 = CARTESIAN_POINT ( 'NONE',  ( 139.6999999999999886, -3659.504999999999654, 2255.774000000000342 ) ) ;
#1781 = DIRECTION ( 'NONE',  ( 0.000000000000000000, -1.000000000000000000, 0.000000000000000000 ) ) ;
#1782 = EDGE_LOOP ( 'NONE', ( #15963, #16432 ) ) ;
#1783 = LINE ( 'NONE', #8929, #16569 ) ;
#1784 = CARTESIAN_POINT ( 'NONE',  ( 72.59320000000001016, -3568.700000000000273, 2239.009999999999764 ) ) ;
#1785 = CARTESIAN_POINT ( 'NONE',  ( 17.56231070083699208, -3576.491783798367123, 2245.815664034199017 ) ) ;
#1786 = DIRECTION ( 'NONE',  ( -1.000000000000000000, 0.000000000000000000, 0.000000000000000000 ) ) ;
#1787 = PERSON_AND_ORGANIZATION ( #5446, #1895 ) ;
#1788 = ORIENTED_EDGE ( 'NONE', *, *, #11296, .T. ) ;
#1789 = VECTOR ( 'NONE', #6465, 1000.000000000000000 ) ;
#1790 = LINE ( 'NONE', #12796, #22343 ) ;
#1791 = DIRECTION ( 'NONE',  ( 1.000000000000000000, 0.000000000000000000, 0.000000000000000000 ) ) ;
#1792 = ORIENTED_EDGE ( 'NONE', *, *, #6294, .T. ) ;
#1793 = CARTESIAN_POINT ( 'NONE',  ( 21.79320000000099711, -3619.500000000000000, 2239.009999999999764 ) ) ;
#1794 = CYLINDRICAL_SURFACE ( 'NONE', #11682, 0.7620000000000000107 ) ;
#1795 = EDGE_CURVE ( 'NONE', #1396, #6791, #16164, .T. ) ;
#1796 = ORIENTED_EDGE ( 'NONE', *, *, #7379, .T. ) ;
#1797 = EDGE_CURVE ( 'NONE', #13900, #7881, #22878, .T. ) ;
#1798 = CARTESIAN_POINT ( 'NONE',  ( 12.69999999999999929, -3653.027999999999793, 2268.705139999999574 ) ) ;
#1799 = ADVANCED_FACE ( 'NONE', ( #5624 ), #20640, .T. ) ;
#1800 = TOROIDAL_SURFACE ( 'NONE', #4406, 3.606799999998999695, 0.7620000000000000107 ) ;
#1801 = ORIENTED_EDGE ( 'NONE', *, *, #7994, .T. ) ;
#1802 = EDGE_LOOP ( 'NONE', ( #12022, #10512, #21670, #1555 ) ) ;
#1803 = EDGE_LOOP ( 'NONE', ( #3126, #6623 ) ) ;
#1804 = CARTESIAN_POINT ( 'NONE',  ( 9.855190710340998805, -3579.429666650000399, 2250.179986546000237 ) ) ;
#1805 = EDGE_LOOP ( 'NONE', ( #15141, #9589 ) ) ;
#1806 = EDGE_LOOP ( 'NONE', ( #975, #14282, #10355 ) ) ;
#1807 = ITEM_DEFINED_TRANSFORMATION ( 'NONE', 'NONE', #2994,  #5611 ) ;
#1808 = SPHERICAL_SURFACE ( 'NONE', #21143, 0.7620000000000000107 ) ;
#1809 = VERTEX_POINT ( 'NONE', #12760 ) ;
#1810 = LINE ( 'NONE', #18092, #1354 ) ;
#1811 = DIRECTION ( 'NONE',  ( 1.000000000000000000, 5.432398939370943590E-28, -2.324635735433000369E-14 ) ) ;
#1812 = DIRECTION ( 'NONE',  ( -1.000000000000000000, 2.330758767201999921E-14, 2.343004830739999973E-14 ) ) ;
#1813 = EDGE_CURVE ( 'NONE', #8599, #17497, #4946, .T. ) ;
#1814 = CARTESIAN_POINT ( 'NONE',  ( 151.4000000000000057, -3543.299999999999727, 2279.827800000000025 ) ) ;
#1815 = PRODUCT_CONTEXT ( 'NONE', #483, 'mechanical' ) ;
#1816 = ORIENTED_EDGE ( 'NONE', *, *, #16841, .T. ) ;
#1817 = CARTESIAN_POINT ( 'NONE',  ( 131.9229944970066413, -3543.650737883654983, 2260.206970375517358 ) ) ;
#1818 = B_SPLINE_CURVE_WITH_KNOTS ( 'NONE', 3,
 ( #19225, #10427, #12068, #14068, #6698, #8330, #12189, #22605, #4806, #20866, #11841, #15822, #17567, #15475, #8452, #6582, #1517, #13723, #11954, #10312, #13950, #15598, #5043, #21099 ),
 .UNSPECIFIED., .F., .F.,
 ( 4, 2, 2, 1, 1, 2, 2, 2, 2, 1, 1, 2, 2, 4 ),
 ( 0.000000000000000000, 0.2499999999966758257, 0.3749999999947900564, 0.4374999999941148743, 0.4687499999937840278, 0.4843749999938956052, 0.4999999999940071271, 0.6249999999889135349, 0.6874999999858730781, 0.7187499999848055987, 0.7343749999842796861, 0.7421874999841302500, 0.7499999999839809250, 1.000000000000000000 ),
 .UNSPECIFIED. ) ;
#1819 = DIRECTION ( 'NONE',  ( 0.000000000000000000, 0.000000000000000000, -1.000000000000000000 ) ) ;
#1820 = ORIENTED_EDGE ( 'NONE', *, *, #18113, .F. ) ;
#1821 = CARTESIAN_POINT ( 'NONE',  ( 139.6999999999999886, -3659.504999999999654, 2272.030000000000200 ) ) ;
#1822 = ORIENTED_EDGE ( 'NONE', *, *, #15713, .F. ) ;
#1823 = FACE_BOUND ( 'NONE', #15815, .T. ) ;
#1824 = CARTESIAN_POINT ( 'NONE',  ( 12.69999999999999929, -3648.710000000000036, 2268.705139999999574 ) ) ;
#1825 = LINE ( 'NONE', #1944, #3225 ) ;
#1826 = B_SPLINE_CURVE_WITH_KNOTS ( 'NONE', 3,
 ( #22448, #6422, #17298, #1246 ),
 .UNSPECIFIED., .F., .F.,
 ( 4, 4 ),
 ( 0.000000000000000000, 1.000000000000000000 ),
 .UNSPECIFIED. ) ;
#1827 = SPHERICAL_SURFACE ( 'NONE', #8869, 1.270000000000000018 ) ;
#1828 = DIRECTION ( 'NONE',  ( -1.000000000000000000, 0.000000000000000000, 0.000000000000000000 ) ) ;
#1829 = ORIENTED_EDGE ( 'NONE', *, *, #6722, .F. ) ;
#1830 = EDGE_CURVE ( 'NONE', #15313, #17962, #22150, .T. ) ;
#1831 = ADVANCED_FACE ( 'NONE', ( #14642 ), #18048, .T. ) ;
#1832 = DIRECTION ( 'NONE',  ( 0.000000000000000000, 0.000000000000000000, 1.000000000000000000 ) ) ;
#1833 = ORIENTED_EDGE ( 'NONE', *, *, #10605, .F. ) ;
#1834 = CYLINDRICAL_SURFACE ( 'NONE', #2773, 3.175000000000149925 ) ;
#1835 = CIRCLE ( 'NONE', #13419, 2.844800000000091700 ) ;
#1836 = DIRECTION ( 'NONE',  ( 0.000000000000000000, -1.000000000000000000, 0.000000000000000000 ) ) ;
#1837 = CYLINDRICAL_SURFACE ( 'NONE', #16065, 0.7619999999999294005 ) ;
#1838 = CARTESIAN_POINT ( 'NONE',  ( 14.50450911876278148, -3657.305732182916017, 2247.637440964547750 ) ) ;
#1839 = FACE_OUTER_BOUND ( 'NONE', #21727, .T. ) ;
#1840 = VERTEX_POINT ( 'NONE', #15931 ) ;
#1841 = EDGE_CURVE ( 'NONE', #22341, #20273, #10934, .T. ) ;
#1842 = CARTESIAN_POINT ( 'NONE',  ( 10.62015369107034424, -3577.553924892425584, 2249.919332792890145 ) ) ;
#1843 = EDGE_LOOP ( 'NONE', ( #9140, #587, #1474, #10656 ) ) ;
#1844 = DIRECTION ( 'NONE',  ( 0.000000000000000000, 0.000000000000000000, -1.000000000000000000 ) ) ;
#1845 = DIRECTION ( 'NONE',  ( 0.000000000000000000, 0.000000000000000000, 1.000000000000000000 ) ) ;
#1846 = APPROVAL_STATUS ( 'not_yet_approved' ) ;
#1847 = EDGE_CURVE ( 'NONE', #21628, #1200, #1864, .T. ) ;
#1848 = TOROIDAL_SURFACE ( 'NONE', #5970, 1.905000000000000027, 1.270000000000000018 ) ;
#1849 = CARTESIAN_POINT ( 'NONE',  ( 12.69999999999999929, -3664.965999999999894, 2239.391000000000076 ) ) ;
#1850 = EDGE_CURVE ( 'NONE', #11364, #15707, #9804, .T. ) ;
#1851 = CARTESIAN_POINT ( 'NONE',  ( 10.49453184711000020, -3657.700682589000280, 2257.813182895999944 ) ) ;
#1852 = CARTESIAN_POINT ( 'NONE',  ( 1.270000000000000018, -3695.699999999999818, 2259.329999999999927 ) ) ;
#1853 = VECTOR ( 'NONE', #12847, 1000.000000000000114 ) ;
#1854 = DIRECTION ( 'NONE',  ( 0.000000000000000000, -1.000000000000000000, 0.000000000000000000 ) ) ;
#1855 = DIRECTION ( 'NONE',  ( -0.5000000000031962211, 0.8660254037825932949, 0.000000000000000000 ) ) ;
#1856 = VERTEX_POINT ( 'NONE', #6194 ) ;
#1857 = CARTESIAN_POINT ( 'NONE',  ( 114.2999999999999972, -3644.899999999999636, 2261.869999999999891 ) ) ;
#1858 = ADVANCED_FACE ( 'NONE', ( #8061 ), #4196, .T. ) ;
#1859 = DIRECTION ( 'NONE',  ( 0.000000000000000000, 0.000000000000000000, -1.000000000000000000 ) ) ;
#1860 = VERTEX_POINT ( 'NONE', #18604 ) ;
#1861 = DIRECTION ( 'NONE',  ( -1.000000000000000000, 0.000000000000000000, 0.000000000000000000 ) ) ;
#1862 = ORIENTED_EDGE ( 'NONE', *, *, #23159, .F. ) ;
#1863 = CARTESIAN_POINT ( 'NONE',  ( 142.3769745404992477, -3695.298184790463893, 2255.430976451231345 ) ) ;
#1864 = LINE ( 'NONE', #11124, #7577 ) ;
#1865 = LOCAL_TIME ( 17, 37, 43.00000000000000000, #16566 ) ;
#1866 = TOROIDAL_SURFACE ( 'NONE', #21327, 3.606799999999999784, 0.7620000000000000107 ) ;
#1867 = ORIENTED_EDGE ( 'NONE', *, *, #22414, .T. ) ;
#1868 = CARTESIAN_POINT ( 'NONE',  ( 137.6222368942718219, -3581.439509223405366, 2248.597413845674510 ) ) ;
#1869 = ORIENTED_EDGE ( 'NONE', *, *, #21910, .T. ) ;
#1870 = DIRECTION ( 'NONE',  ( 0.000000000000000000, 1.000000000000000000, 0.000000000000000000 ) ) ;
#1871 = COORDINATED_UNIVERSAL_TIME_OFFSET ( 0, 0, .AHEAD. ) ;
#1872 = DIRECTION ( 'NONE',  ( -1.000000000000000000, 0.000000000000000000, 0.000000000000000000 ) ) ;
#1873 = DIRECTION ( 'NONE',  ( 0.000000000000000000, -1.000000000000000000, 0.000000000000000000 ) ) ;
#1874 = CIRCLE ( 'NONE', #7493, 3.606799999999993567 ) ;
#1875 = DIRECTION ( 'NONE',  ( -0.8660254037820785955, -0.5000000000040877302, 3.192239903039919200E-14 ) ) ;
#1876 = DIRECTION ( 'NONE',  ( 0.000000000000000000, -1.000000000000000000, 0.000000000000000000 ) ) ;
#1877 = APPLIED_SECURITY_CLASSIFICATION_ASSIGNMENT ( #4122, ( #7485 ) ) ;
#1878 = CARTESIAN_POINT ( 'NONE',  ( 140.6533150761702586, -3576.814124183825697, 2249.368845734366005 ) ) ;
#1879 = ORIENTED_EDGE ( 'NONE', *, *, #16323, .T. ) ;
#1880 = CARTESIAN_POINT ( 'NONE',  ( 134.6950185071150088, -3576.735968958820195, 2245.499284827320935 ) ) ;
#1881 = CARTESIAN_POINT ( 'NONE',  ( 15.54479972196000048, -3579.403078500999982, 2257.962943248000101 ) ) ;
#1882 = VERTEX_POINT ( 'NONE', #7597 ) ;
#1883 = DIRECTION ( 'NONE',  ( 0.000000000000000000, 0.000000000000000000, 1.000000000000000000 ) ) ;
#1884 = DIRECTION ( 'NONE',  ( 0.000000000000000000, -1.000000000000000000, 0.000000000000000000 ) ) ;
#1885 = APPROVAL ( #1846, 'UNKNOWN' ) ;
#1886 = EDGE_LOOP ( 'NONE', ( #12243, #7202, #17473, #20445 ) ) ;
#1887 = CARTESIAN_POINT ( 'NONE',  ( 133.9849999999999852, -3659.504999999999654, 2246.630000000000109 ) ) ;
#1888 = FACE_OUTER_BOUND ( 'NONE', #14803, .T. ) ;
#1889 = ORIENTED_EDGE ( 'NONE', *, *, #21889, .F. ) ;
#1890 = LINE ( 'NONE', #5651, #17316 ) ;
#1891 = CARTESIAN_POINT ( 'NONE',  ( 12.69997737250858982, -3642.347301253999831, 2279.817639304488239 ) ) ;
#1892 = EDGE_CURVE ( 'NONE', #2232, #15313, #4213, .T. ) ;
#1893 = LOCAL_TIME ( 17, 37, 43.00000000000000000, #16054 ) ;
#1894 = DIRECTION ( 'NONE',  ( -2.324635735433000053E-14, 2.336881798971000105E-14, -1.000000000000000000 ) ) ;
#1895 = ORGANIZATION ( 'UNSPECIFIED', 'UNSPECIFIED', '' ) ;
#1896 = PLANE ( 'NONE',  #19362 ) ;
#1897 = PERSON_AND_ORGANIZATION ( #5446, #1895 ) ;
#1898 = ORIENTED_EDGE ( 'NONE', *, *, #20590, .F. ) ;
#1899 = AXIS2_PLACEMENT_3D ( 'NONE', #23040, #8324, #3360 ) ;
#1900 = CARTESIAN_POINT ( 'NONE',  ( 137.2104978356082938, -3660.942314744984742, 2239.009999999967931 ) ) ;
#1901 = CARTESIAN_POINT ( 'NONE',  ( 151.4000000000000057, 0.000000000000000000, 0.000000000000000000 ) ) ;
#1902 = ORIENTED_EDGE ( 'NONE', *, *, #10950, .T. ) ;
#1903 = CARTESIAN_POINT ( 'NONE',  ( 18.12377227050810546, -3581.296112607328268, 2245.922901418339279 ) ) ;
#1904 = CARTESIAN_POINT ( 'NONE',  ( 95.25000000000000000, -3670.300000000000182, 2247.392000000000280 ) ) ;
#1905 = CIRCLE ( 'NONE', #20993, 5.715000000000872937 ) ;
#1906 = VERTEX_POINT ( 'NONE', #2553 ) ;
#1907 = VERTEX_POINT ( 'NONE', #15209 ) ;
#1908 = CARTESIAN_POINT ( 'NONE',  ( 137.7820634117503573, -3661.606662391098325, 2249.829843942283787 ) ) ;
#1909 = ORIENTED_EDGE ( 'NONE', *, *, #918, .T. ) ;
#1910 = ORIENTED_EDGE ( 'NONE', *, *, #16604, .F. ) ;
#1911 = APPLIED_SECURITY_CLASSIFICATION_ASSIGNMENT ( #3396, ( #23173 ) ) ;
#1912 = APPLIED_SECURITY_CLASSIFICATION_ASSIGNMENT ( #13135, ( #12017 ) ) ;
#1913 = ORIENTED_EDGE ( 'NONE', *, *, #14986, .T. ) ;
#1914 = APPLIED_PERSON_AND_ORGANIZATION_ASSIGNMENT ( #21278, #12362, ( #3194 ) ) ;
#1915 = CARTESIAN_POINT ( 'NONE',  ( -12.31900000000000084, -3576.167599999999766, 2247.392000000000280 ) ) ;
#1916 = EDGE_LOOP ( 'NONE', ( #12690, #14299, #22719, #12758, #21325, #19968 ) ) ;
#1917 = ORIENTED_EDGE ( 'NONE', *, *, #22733, .F. ) ;
#1918 = DIRECTION ( 'NONE',  ( 0.000000000000000000, 0.000000000000000000, 1.000000000000000000 ) ) ;
#1919 = PERSON_AND_ORGANIZATION ( #703, #18745 ) ;
#1920 = PLANE ( 'NONE',  #10661 ) ;
#1921 = AXIS2_PLACEMENT_3D ( 'NONE', #21651, #8883, #3947 ) ;
#1922 = FACE_OUTER_BOUND ( 'NONE', #4676, .T. ) ;
#1923 = VERTEX_POINT ( 'NONE', #6082 ) ;
#1924 = VECTOR ( 'NONE', #3908, 1000.000000000000114 ) ;
#1925 = DIRECTION ( 'NONE',  ( 0.000000000000000000, 0.000000000000000000, -1.000000000000000000 ) ) ;
#1926 = EDGE_CURVE ( 'NONE', #5052, #15577, #13332, .T. ) ;
#1927 = FACE_BOUND ( 'NONE', #9861, .T. ) ;
#1928 = DIRECTION ( 'NONE',  ( 0.000000000000000000, 0.000000000000000000, 1.000000000000000000 ) ) ;
#1929 = ADVANCED_FACE ( 'NONE', ( #7830 ), #5968, .T. ) ;
#1930 = CARTESIAN_POINT ( 'NONE',  ( 12.69999999999999929, -3639.502500000000055, 2288.971800000000258 ) ) ;
#1931 = SHAPE_DEFINITION_REPRESENTATION ( #19683, #21348 ) ;
#1932 = EDGE_CURVE ( 'NONE', #21382, #14294, #18786, .T. ) ;
#1933 = EDGE_LOOP ( 'NONE', ( #7935, #18897, #1571, #14077 ) ) ;
#1934 = CARTESIAN_POINT ( 'NONE',  ( 9.855190710340998805, -3579.495000415000050, 2250.165025612000136 ) ) ;
#1935 = EDGE_LOOP ( 'NONE', ( #6565, #20675, #8274, #261 ) ) ;
#1936 = CYLINDRICAL_SURFACE ( 'NONE', #10928, 0.3810000000000746678 ) ;
#1937 = DIRECTION ( 'NONE',  ( 0.000000000000000000, -1.000000000000000000, 0.000000000000000000 ) ) ;
#1938 = EDGE_LOOP ( 'NONE', ( #1559, #5914, #14362, #3986 ) ) ;
#1939 = AXIS2_PLACEMENT_3D ( 'NONE', #6032, #848, #21956 ) ;
#1940 = CARTESIAN_POINT ( 'NONE',  ( 151.4000000000000057, -3544.061999999999898, 2295.829799999999977 ) ) ;
#1941 = VECTOR ( 'NONE', #18173, 1000.000000000000000 ) ;
#1942 = EDGE_CURVE ( 'NONE', #15342, #6713, #6833, .T. ) ;
#1943 = DIRECTION ( 'NONE',  ( 0.000000000000000000, 0.000000000000000000, 1.000000000000000000 ) ) ;
#1944 = CARTESIAN_POINT ( 'NONE',  ( 151.1299999999999955, -3544.570000000000164, 2239.009999999999764 ) ) ;
#1945 = CARTESIAN_POINT ( 'NONE',  ( 91.74479999999999791, -3594.099999999999909, 2259.837999999999738 ) ) ;
#1946 = CYLINDRICAL_SURFACE ( 'NONE', #20025, 3.175000000000149925 ) ;
#1947 = CARTESIAN_POINT ( 'NONE',  ( 147.6742428626672563, -3543.355825688684035, 2259.712068108529820 ) ) ;
#1948 = EDGE_LOOP ( 'NONE', ( #13258, #3240, #10560, #10064 ) ) ;
#1949 = CARTESIAN_POINT ( 'NONE',  ( 147.8270794805000037, -3695.699999999999818, 2259.329999999999927 ) ) ;
#1950 = DIRECTION ( 'NONE',  ( 0.000000000000000000, 0.000000000000000000, 1.000000000000000000 ) ) ;
#1951 = CARTESIAN_POINT ( 'NONE',  ( 57.14999999999999858, -3544.570000000000164, 2243.277199999999993 ) ) ;
#1952 = DIRECTION ( 'NONE',  ( 0.000000000000000000, 0.000000000000000000, -1.000000000000000000 ) ) ;
#1953 = CARTESIAN_POINT ( 'NONE',  ( 142.5418842717801340, -3543.408637598919540, 2255.017974340328692 ) ) ;
#1954 = DIRECTION ( 'NONE',  ( 0.000000000000000000, 0.000000000000000000, -1.000000000000000000 ) ) ;
#1955 = AXIS2_PLACEMENT_3D ( 'NONE', #6196, #1020, #11459 ) ;
#1956 = VECTOR ( 'NONE', #8650, 1000.000000000000000 ) ;
#1957 = CARTESIAN_POINT ( 'NONE',  ( 7.430466206498319792, -3577.282607159902909, 2245.023857075259002 ) ) ;
#1958 = VERTEX_POINT ( 'NONE', #22340 ) ;
#1959 = PERSON_AND_ORGANIZATION_ROLE ( 'creator' ) ;
#1960 = EDGE_CURVE ( 'NONE', #20500, #8369, #22528, .T. ) ;
#1961 = AXIS2_PLACEMENT_3D ( 'NONE', #7484, #7261, #9252 ) ;
#1962 = DIRECTION ( 'NONE',  ( 0.000000000000000000, 0.000000000000000000, 1.000000000000000000 ) ) ;
#1963 = DIRECTION ( 'NONE',  ( 0.000000000000000000, 1.000000000000000000, 0.000000000000000000 ) ) ;
#1964 = COORDINATED_UNIVERSAL_TIME_OFFSET ( 0, 0, .AHEAD. ) ;
#1965 = EDGE_CURVE ( 'NONE', #11744, #3669, #1203, .T. ) ;
#1966 = LINE ( 'NONE', #7469, #16553 ) ;
#1967 = EDGE_CURVE ( 'NONE', #21948, #140, #105, .T. ) ;
#1968 = LINE ( 'NONE', #15683, #2618 ) ;
#1969 = CARTESIAN_POINT ( 'NONE',  ( 151.3999999999999773, -3543.329032635400836, 2240.279999999999745 ) ) ;
#1970 = TOROIDAL_SURFACE ( 'NONE', #16185, 5.588000000000000078, 0.7620000000000000107 ) ;
#1971 = DIRECTION ( 'NONE',  ( 0.000000000000000000, 0.000000000000000000, 1.000000000000000000 ) ) ;
#1972 = VECTOR ( 'NONE', #3362, 1000.000000000000000 ) ;
#1973 = ORIENTED_EDGE ( 'NONE', *, *, #16267, .T. ) ;
#1974 = CARTESIAN_POINT ( 'NONE',  ( 3.048000000000000043, -3695.699999999999818, 2229.612000000000080 ) ) ;
#1975 = ORIENTED_EDGE ( 'NONE', *, *, #14228, .T. ) ;
#1976 = VECTOR ( 'NONE', #8637, 1000.000000000000000 ) ;
#1977 = CARTESIAN_POINT ( 'NONE',  ( 101.5999999999999943, -3568.700000000000273, 2239.771999999999935 ) ) ;
#1978 = AXIS2_PLACEMENT_3D ( 'NONE', #20945, #19307, #6893 ) ;
#1979 = CARTESIAN_POINT ( 'NONE',  ( 10.28147353980999945, -3637.993101834000299, 2279.551731614000346 ) ) ;
#1980 = ORIENTED_EDGE ( 'NONE', *, *, #3904, .T. ) ;
#1981 = DIRECTION ( 'NONE',  ( 0.000000000000000000, 0.000000000000000000, -1.000000000000000000 ) ) ;
#1982 = EDGE_CURVE ( 'NONE', #2186, #17917, #3455, .T. ) ;
#1983 = ORIENTED_EDGE ( 'NONE', *, *, #16023, .F. ) ;
#1984 = DIRECTION ( 'NONE',  ( 0.000000000000000000, 0.000000000000000000, -1.000000000000000000 ) ) ;
#1985 = CIRCLE ( 'NONE', #10963, 5.715000000000001634 ) ;
#1986 = ORIENTED_EDGE ( 'NONE', *, *, #18297, .T. ) ;
#1987 = CARTESIAN_POINT ( 'NONE',  ( 137.8755860065629975, -3581.677971386929130, 2247.791257809596118 ) ) ;
#1988 = EDGE_LOOP ( 'NONE', ( #9422, #22427 ) ) ;
#1990 = FACE_OUTER_BOUND ( 'NONE', #22130, .T. ) ;
#1989 = VECTOR ( 'NONE', #2955, 1000.000000000000000 ) ;
#1991 = PERSON_AND_ORGANIZATION ( #5446, #1895 ) ;
#1992 = AXIS2_PLACEMENT_3D ( 'NONE', #21698, #2245, #18064 ) ;
#1993 = APPLICATION_CONTEXT ( 'configuration controlled 3d designs of mechanical parts and assemblies' ) ;
#1994 = ADVANCED_FACE ( 'NONE', ( #13443 ), #5859, .F. ) ;
#1995 = CARTESIAN_POINT ( 'NONE',  ( 6.985000002048999512, -3579.494756921999851, 2244.617465693000213 ) ) ;
#1996 = CYLINDRICAL_SURFACE ( 'NONE', #13744, 5.714999999999998082 ) ;
#1997 = DIRECTION ( 'NONE',  ( 3.028227728875025183E-14, 0.5000000000049040771, 0.8660254037816071948 ) ) ;
#1998 = DIRECTION ( 'NONE',  ( 0.000000000000000000, 0.000000000000000000, 1.000000000000000000 ) ) ;
#1999 = CARTESIAN_POINT ( 'NONE',  ( 141.1782708254342822, -3577.063961468278649, 2249.598379591055163 ) ) ;
#2000 = VERTEX_POINT ( 'NONE', #11562 ) ;
#2001 = CIRCLE ( 'NONE', #5370, 2.844800000000091700 ) ;
#2002 = CARTESIAN_POINT ( 'NONE',  ( 135.0631415578579606, -3576.153948019764357, 2246.504844866586154 ) ) ;
#2003 = CARTESIAN_POINT ( 'NONE',  ( 6.985000000000999520, -3599.497499999999945, 2288.971800000000258 ) ) ;
#2004 = ORIENTED_EDGE ( 'NONE', *, *, #11208, .T. ) ;
#2005 = CARTESIAN_POINT ( 'NONE',  ( 139.6999999999999886, -3662.197400000000016, 2242.820000000000164 ) ) ;
#2006 = CARTESIAN_POINT ( 'NONE',  ( 139.7000000001000046, -3656.812599999999748, 2242.820000000000164 ) ) ;
#2007 = EDGE_CURVE ( 'NONE', #13971, #19453, #4084, .T. ) ;
#2008 = AXIS2_PLACEMENT_3D ( 'NONE', #13031, #20176, #4116 ) ;
#2009 = EDGE_CURVE ( 'NONE', #22481, #18295, #3084, .T. ) ;
#2010 = AXIS2_PLACEMENT_3D ( 'NONE', #12669, #259, #11022 ) ;
#2011 = EDGE_LOOP ( 'NONE', ( #22425, #17935, #19349, #11921 ) ) ;
#2012 = DIRECTION ( 'NONE',  ( 1.000000000000000000, 0.000000000000000000, 0.000000000000000000 ) ) ;
#2013 = PLANE ( 'NONE',  #2455 ) ;
#2014 = EDGE_LOOP ( 'NONE', ( #20946, #5388 ) ) ;
#2015 = DIRECTION ( 'NONE',  ( 1.000000000000000000, 0.000000000000000000, 0.000000000000000000 ) ) ;
#2016 = PLANE ( 'NONE',  #20971 ) ;
#2017 = FACE_OUTER_BOUND ( 'NONE', #15289, .T. ) ;
#2018 = CARTESIAN_POINT ( 'NONE',  ( 10.36831320292846925, -3660.851200000039626, 2239.391000000000076 ) ) ;
#2019 = AXIS2_PLACEMENT_3D ( 'NONE', #17462, #22736, #15605 ) ;
#2020 = APPROVAL_STATUS ( 'not_yet_approved' ) ;
#2021 = EDGE_LOOP ( 'NONE', ( #17301, #1062 ) ) ;
#2022 = DIRECTION ( 'NONE',  ( 0.000000000000000000, 1.000000000000000000, 0.000000000000000000 ) ) ;
#2023 = DIRECTION ( 'NONE',  ( 0.000000000000000000, 0.000000000000000000, 1.000000000000000000 ) ) ;
#2024 = VERTEX_POINT ( 'NONE', #9363 ) ;
#2025 = CARTESIAN_POINT ( 'NONE',  ( 18.26136626118261574, -3580.811168666933554, 2245.321774183003981 ) ) ;
#2026 = CARTESIAN_POINT ( 'NONE',  ( 137.3727324534160914, -3657.868512552856373, 2249.105625754800258 ) ) ;
#2027 = VERTEX_POINT ( 'NONE', #9473 ) ;
#2028 = VERTEX_POINT ( 'NONE', #16615 ) ;
#2029 = CARTESIAN_POINT ( 'NONE',  ( 141.5159261927328487, -3661.696737588060842, 2249.774008737822442 ) ) ;
#2030 = EDGE_LOOP ( 'NONE', ( #18560, #22944, #14148, #10652, #19150, #6316, #6195, #22525 ) ) ;
#2031 = ORIENTED_EDGE ( 'NONE', *, *, #4855, .T. ) ;
#2032 = CIRCLE ( 'NONE', #9864, 3.606800000000000228 ) ;
#2033 = DIRECTION ( 'NONE',  ( 0.8660254037841628172, -0.5000000000004778400, 0.000000000000000000 ) ) ;
#2034 = VECTOR ( 'NONE', #13795, 1000.000000000000000 ) ;
#2035 = ORIENTED_EDGE ( 'NONE', *, *, #503, .F. ) ;
#2036 = EDGE_LOOP ( 'NONE', ( #17370, #5477 ) ) ;
#2037 = CARTESIAN_POINT ( 'NONE',  ( 15.44319999999931525, -3658.626742952524637, 2255.967040000000907 ) ) ;
#2038 = DATE_TIME_ROLE ( 'classification_date' ) ;
#2039 = CYLINDRICAL_SURFACE ( 'NONE', #5814, 0.3809999999999924558 ) ;
#2040 = DIRECTION ( 'NONE',  ( 0.000000000000000000, 0.000000000000000000, 1.000000000000000000 ) ) ;
#2041 = ORIENTED_EDGE ( 'NONE', *, *, #6288, .F. ) ;
#2042 = CARTESIAN_POINT ( 'NONE',  ( 142.4126867972000241, -3577.928829547000078, 2239.009999999999764 ) ) ;
#2043 = DIRECTION ( 'NONE',  ( 0.000000000000000000, -1.000000000000000000, 0.000000000000000000 ) ) ;
#2044 = CARTESIAN_POINT ( 'NONE',  ( 7.322952892593269425, -3581.431939765986954, 2246.174326570242556 ) ) ;
#2045 = DIRECTION ( 'NONE',  ( -1.000000000000000000, 0.000000000000000000, 0.000000000000000000 ) ) ;
#2046 = SECURITY_CLASSIFICATION_LEVEL ( 'unclassified' ) ;
#2047 = DIRECTION ( 'NONE',  ( 0.000000000000000000, -1.000000000000000000, 0.000000000000000000 ) ) ;
#2048 = ORIENTED_EDGE ( 'NONE', *, *, #20807, .T. ) ;
#2049 = VECTOR ( 'NONE', #17052, 1000.000000000000000 ) ;
#2050 = APPLIED_PERSON_AND_ORGANIZATION_ASSIGNMENT ( #9754, #633, ( #6959 ) ) ;
#2051 = AXIS2_PLACEMENT_3D ( 'NONE', #22075, #2404, #16693 ) ;
#2052 = CARTESIAN_POINT ( 'NONE',  ( -12.31900000000000084, -3581.209255678999853, 2246.035656601000028 ) ) ;
#2053 = ORIENTED_EDGE ( 'NONE', *, *, #22020, .T. ) ;
#2054 = ADVANCED_FACE ( 'NONE', ( #2444 ), #682, .F. ) ;
#2055 = CARTESIAN_POINT ( 'NONE',  ( 28.24479999999899604, -3619.500000000000000, 2259.837999999999738 ) ) ;
#2056 = VECTOR ( 'NONE', #21267, 1000.000000000000000 ) ;
#2057 = DIRECTION ( 'NONE',  ( 0.000000000000000000, 1.000000000000000000, 0.000000000000000000 ) ) ;
#2058 = VERTEX_POINT ( 'NONE', #4314 ) ;
#2059 = CARTESIAN_POINT ( 'NONE',  ( 57.14999999999999858, -3670.300000000000182, 2247.392000000000280 ) ) ;
#2060 = EDGE_CURVE ( 'NONE', #279, #16346, #14693, .T. ) ;
#2061 = ADVANCED_FACE ( 'NONE', ( #13914 ), #17067, .F. ) ;
#2062 = DIRECTION ( 'NONE',  ( 0.000000000000000000, 0.000000000000000000, 1.000000000000000000 ) ) ;
#2063 = CARTESIAN_POINT ( 'NONE',  ( 139.6999999999999886, -3659.504999999999654, 2239.009999999999764 ) ) ;
#2064 = PLANE ( 'NONE',  #11030 ) ;
#2066 = ORIENTED_EDGE ( 'NONE', *, *, #19760, .T. ) ;
#2065 = EDGE_CURVE ( 'NONE', #2024, #2236, #13801, .T. ) ;
#2067 = VERTEX_POINT ( 'NONE', #6774 ) ;
#2068 = CARTESIAN_POINT ( 'NONE',  ( 50.79999999999999716, -3670.300000000000182, 2259.837999999999738 ) ) ;
#2069 = VECTOR ( 'NONE', #2033, 999.9999999999998863 ) ;
#2070 = B_SPLINE_CURVE_WITH_KNOTS ( 'NONE', 3,
 ( #10430, #6927, #8794, #17571, #1521, #6701, #8569, #8679, #22956, #15942, #14072, #11957, #15827, #19229, #23073, #14194, #17336, #13954, #12314, #21224, #4926, #5173, #7050, #21336, #11844, #19110, #18997, #3163, #2939, #20986, #10076, #17222, #1167, #8334, #10316, #15711, #22841, #6585, #12073, #3047, #15478, #10198, #13726 ),
 .UNSPECIFIED., .F., .F.,
 ( 4, 2, 2, 1, 1, 2, 2, 2, 1, 2, 2, 2, 2, 2, 2, 2, 2, 2, 2, 2, 2, 2, 4 ),
 ( 0.000000000000000000, 0.1249999999996564692, 0.1874999999994266253, 0.2187499999993604283, 0.2343749999993274824, 0.2421874999993110233, 0.2499999999992945365, 0.3124999999992997823, 0.3437499999992194577, 0.3593749999991818767, 0.3749999999991442956, 0.4374999999991522337, 0.4687499999992162381, 0.4999999999992802424, 0.5624999999995130562, 0.5937499999996295186, 0.6093749999995666800, 0.6249999999995037303, 0.6874999999994484412, 0.7187499999995694555, 0.7499999999996904698, 0.8749999999998452349, 1.000000000000000000 ),
 .UNSPECIFIED. ) ;
#2071 = FACE_OUTER_BOUND ( 'NONE', #20364, .T. ) ;
#2072 = VECTOR ( 'NONE', #19583, 1000.000000000000000 ) ;
#2073 = CARTESIAN_POINT ( 'NONE',  ( 12.69999999999999929, -3653.789999999999964, 2268.705139999999574 ) ) ;
#2074 = AXIS2_PLACEMENT_3D ( 'NONE', #5740, #11334, #11119 ) ;
#2075 = CARTESIAN_POINT ( 'NONE',  ( -12.31900000000001505, -3658.793799999857129, 2249.723686796825405 ) ) ;
#2076 = CIRCLE ( 'NONE', #5831, 1.269999999999882334 ) ;
#2077 = CARTESIAN_POINT ( 'NONE',  ( 142.2882464502881703, -3544.023782197908986, 2255.653245238742784 ) ) ;
#2078 = EDGE_CURVE ( 'NONE', #2568, #6304, #10195, .T. ) ;
#2079 = CARTESIAN_POINT ( 'NONE',  ( 137.1349041368046073, -3694.826579460890571, 2255.711176449251980 ) ) ;
#2080 = CARTESIAN_POINT ( 'NONE',  ( 7.790018067753250897, -3576.570178142666919, 2245.703553554133578 ) ) ;
#2081 = ORIENTED_EDGE ( 'NONE', *, *, #18439, .T. ) ;
#2082 = APPLICATION_PROTOCOL_DEFINITION ( 'international standard', 'automotive_design', 2000, #11555 ) ;
#2083 = CARTESIAN_POINT ( 'NONE',  ( 127.0000000000000000, -3568.700000000000273, 2239.771999999999935 ) ) ;
#2084 = EDGE_CURVE ( 'NONE', #796, #185, #1248, .T. ) ;
#2085 = FACE_OUTER_BOUND ( 'NONE', #19880, .T. ) ;
#2086 = COORDINATED_UNIVERSAL_TIME_OFFSET ( 0, 0, .AHEAD. ) ;
#2087 = CARTESIAN_POINT ( 'NONE',  ( 101.5999999999999943, -3568.700000000000273, 2239.771999999999935 ) ) ;
#2088 = DIRECTION ( 'NONE',  ( -1.000000000000000000, 0.000000000000000000, 0.000000000000000000 ) ) ;
#2089 = CIRCLE ( 'NONE', #15918, 3.175000000000149925 ) ;
#2090 = CIRCLE ( 'NONE', #17035, 0.7619999999999294005 ) ;
#2091 = DIRECTION ( 'NONE',  ( 2.336881798971000105E-14, 0.000000000000000000, 1.000000000000000000 ) ) ;
#2092 = CIRCLE ( 'NONE', #3956, 7.111999999999785160 ) ;
#2093 = ADVANCED_FACE ( 'NONE', ( #15324 ), #10394, .T. ) ;
#2094 = VERTEX_POINT ( 'NONE', #17300 ) ;
#2095 = CARTESIAN_POINT ( 'NONE',  ( 22.55520000000100111, -3619.500000000000000, 2239.771999999999935 ) ) ;
#2096 = EDGE_LOOP ( 'NONE', ( #19011, #14789, #7651, #15840 ) ) ;
#2097 = AXIS2_PLACEMENT_3D ( 'NONE', #17228, #13486, #2943 ) ;
#2098 = EDGE_CURVE ( 'NONE', #833, #9227, #19190, .T. ) ;
#2099 = CARTESIAN_POINT ( 'NONE',  ( 35.25520000000000209, -3594.099999999999909, 2239.771999999999935 ) ) ;
#2100 = EDGE_CURVE ( 'NONE', #10158, #3298, #5011, .T. ) ;
#2101 = CARTESIAN_POINT ( 'NONE',  ( 12.38520902594999917, -3636.669321837000098, 2279.814656244000162 ) ) ;
#2102 = VERTEX_POINT ( 'NONE', #22799 ) ;
#2103 = CYLINDRICAL_SURFACE ( 'NONE', #8446, 3.175000000000149925 ) ;
#2104 = ORIENTED_EDGE ( 'NONE', *, *, #896, .F. ) ;
#2105 = LINE ( 'NONE', #20031, #16052 ) ;
#2106 = CARTESIAN_POINT ( 'NONE',  ( 64.76999999999999602, -3695.699999999999818, 2292.819899999999961 ) ) ;
#2107 = AXIS2_PLACEMENT_3D ( 'NONE', #23144, #22913, #12497 ) ;
#2108 = VECTOR ( 'NONE', #18026, 1000.000000000000000 ) ;
#2109 = ORIENTED_EDGE ( 'NONE', *, *, #369, .F. ) ;
#2110 = TOROIDAL_SURFACE ( 'NONE', #17803, 3.606799999998999695, 0.7620000000000000107 ) ;
#2111 = CARTESIAN_POINT ( 'NONE',  ( 137.0429226604888697, -3580.511331052818605, 2249.708490802025153 ) ) ;
#2112 = ORIENTED_EDGE ( 'NONE', *, *, #22032, .T. ) ;
#2113 = CARTESIAN_POINT ( 'NONE',  ( 15.41268679728733915, -3657.938829547220848, 2239.009999999999764 ) ) ;
#2114 = APPROVAL_ROLE ( '' ) ;
#2115 = CARTESIAN_POINT ( 'NONE',  ( 133.9850000019999925, -3579.494756921999851, 2244.617465693000213 ) ) ;
#2116 = CYLINDRICAL_SURFACE ( 'NONE', #641, 0.3809999999999924558 ) ;
#2117 = DIRECTION ( 'NONE',  ( 0.5000000000043351989, -0.8660254037819355988, 0.000000000000000000 ) ) ;
#2118 = CARTESIAN_POINT ( 'NONE',  ( 9.903987878842999137, -3578.946623412000008, 2257.950097015999745 ) ) ;
#2119 = DIRECTION ( 'NONE',  ( 0.000000000000000000, 0.000000000000000000, 1.000000000000000000 ) ) ;
#2120 = VERTEX_POINT ( 'NONE', #6424 ) ;
#2121 = CARTESIAN_POINT ( 'NONE',  ( 134.4205046047358110, -3577.301034214552146, 2245.005495992568740 ) ) ;
#2122 = AXIS2_PLACEMENT_3D ( 'NONE', #20201, #18891, #8126 ) ;
#2123 = FACE_OUTER_BOUND ( 'NONE', #18740, .T. ) ;
#2124 = ORIENTED_EDGE ( 'NONE', *, *, #20266, .T. ) ;
#2125 = CARTESIAN_POINT ( 'NONE',  ( 10.32639513556999944, -3581.071539618999850, 2257.848705702999723 ) ) ;
#2126 = CIRCLE ( 'NONE', #9291, 2.844800000000091700 ) ;
#2127 = CARTESIAN_POINT ( 'NONE',  ( 97.99320000000000164, -3568.700000000000273, 2239.009999999999764 ) ) ;
#2128 = EDGE_CURVE ( 'NONE', #19405, #9540, #6099, .T. ) ;
#2129 = AXIS2_PLACEMENT_3D ( 'NONE', #17400, #5234, #15666 ) ;
#2130 = EDGE_LOOP ( 'NONE', ( #2406, #19171, #16491, #20611 ) ) ;
#2131 = EDGE_CURVE ( 'NONE', #18714, #22886, #9455, .T. ) ;
#2132 = CARTESIAN_POINT ( 'NONE',  ( 15.42948858069999929, -3660.322618741000042, 2257.932964559000084 ) ) ;
#2133 = DIRECTION ( 'NONE',  ( 0.000000000000000000, -1.000000000000000000, 4.457650181899999573E-12 ) ) ;
#2134 = ORIENTED_EDGE ( 'NONE', *, *, #9935, .F. ) ;
#2135 = CARTESIAN_POINT ( 'NONE',  ( 86.05520000000001346, -3644.899999999999636, 2239.771999999999935 ) ) ;
#2136 = DIRECTION ( 'NONE',  ( 0.8928571428588499836, -0.4503400076008471919, 0.000000000000000000 ) ) ;
#2137 = FACE_OUTER_BOUND ( 'NONE', #1043, .T. ) ;
#2138 = EDGE_CURVE ( 'NONE', #3607, #17982, #10040, .T. ) ;
#2139 = ORIENTED_EDGE ( 'NONE', *, *, #14366, .F. ) ;
#2140 = VECTOR ( 'NONE', #276, 1000.000000000000000 ) ;
#2141 = CARTESIAN_POINT ( 'NONE',  ( 137.3683132029000262, -3658.158799999999701, 2242.820000000000164 ) ) ;
#2142 = COORDINATED_UNIVERSAL_TIME_OFFSET ( 0, 0, .AHEAD. ) ;
#2143 = AXIS2_PLACEMENT_3D ( 'NONE', #21953, #3683, #18096 ) ;
#2144 = DIRECTION ( 'NONE',  ( 0.000000000000000000, 0.000000000000000000, -1.000000000000000000 ) ) ;
#2145 = CARTESIAN_POINT ( 'NONE',  ( 139.6999999999999886, -3579.494999999999891, 2272.030000000000200 ) ) ;
#2146 = VERTEX_POINT ( 'NONE', #4884 ) ;
#2147 = FACE_OUTER_BOUND ( 'NONE', #19239, .T. ) ;
#2148 = ADVANCED_FACE ( 'NONE', ( #15788 ), #22572, .F. ) ;
#2149 = CARTESIAN_POINT ( 'NONE',  ( 137.9086613251612050, -3657.294972066808896, 2247.463768499330854 ) ) ;
#2150 = EDGE_CURVE ( 'NONE', #1650, #5650, #1582, .T. ) ;
#2151 = EDGE_LOOP ( 'NONE', ( #20970, #18599, #20729, #22992 ) ) ;
#2152 = VECTOR ( 'NONE', #4453, 1000.000000000000000 ) ;
#2153 = ORIENTED_EDGE ( 'NONE', *, *, #20313, .T. ) ;
#2154 = CARTESIAN_POINT ( 'NONE',  ( 138.6914917811226644, -3662.165394498078058, 2249.389780753679133 ) ) ;
#2155 = EDGE_LOOP ( 'NONE', ( #7599, #8779, #13413, #12237 ) ) ;
#2156 = ORIENTED_EDGE ( 'NONE', *, *, #14228, .F. ) ;
#2157 = AXIS2_PLACEMENT_3D ( 'NONE', #14536, #3859, #17918 ) ;
#2158 = EDGE_CURVE ( 'NONE', #3136, #20114, #8191, .T. ) ;
#2159 = CARTESIAN_POINT ( 'NONE',  ( 9.855201422231997910, -3599.497499926000273, 2279.447341858000073 ) ) ;
#2160 = VERTEX_POINT ( 'NONE', #8290 ) ;
#2161 = VERTEX_POINT ( 'NONE', #6544 ) ;
#2162 = DIRECTION ( 'NONE',  ( -1.000000000000000000, 0.000000000000000000, 0.000000000000000000 ) ) ;
#2163 = APPROVAL_DATE_TIME ( #13049, #17193 ) ;
#2164 = DIRECTION ( 'NONE',  ( 0.000000000000000000, 0.000000000000000000, 1.000000000000000000 ) ) ;
#2165 = ORIENTED_EDGE ( 'NONE', *, *, #17307, .F. ) ;
#2166 = AXIS2_PLACEMENT_3D ( 'NONE', #16151, #10405, #17546 ) ;
#2167 = LINE ( 'NONE', #3680, #8110 ) ;
#2168 = CIRCLE ( 'NONE', #21251, 0.7620000000000126672 ) ;
#2169 = LINE ( 'NONE', #15042, #9720 ) ;
#2170 = CARTESIAN_POINT ( 'NONE',  ( 22.54063073453000143, -3544.061999999999898, 2275.763800000000174 ) ) ;
#2171 = DIRECTION ( 'NONE',  ( 0.000000000000000000, 0.000000000000000000, 1.000000000000000000 ) ) ;
#2172 = PERSON_AND_ORGANIZATION ( #5446, #1895 ) ;
#2173 =( REPRESENTATION_RELATIONSHIP ('NONE','NONE', #20448, #5332 ) REPRESENTATION_RELATIONSHIP_WITH_TRANSFORMATION ( #5912 )SHAPE_REPRESENTATION_RELATIONSHIP( ) );
#2174 = DIRECTION ( 'NONE',  ( 0.6887494619146540265, 0.000000000000000000, -0.7249994335944508483 ) ) ;
#2175 = CARTESIAN_POINT ( 'NONE',  ( 12.69999999999999929, -3599.497499999999945, 2295.829799999999977 ) ) ;
#2176 = AXIS2_PLACEMENT_3D ( 'NONE', #9993, #4724, #6377 ) ;
#2177 = LINE ( 'NONE', #9322, #8912 ) ;
#2178 = FACE_OUTER_BOUND ( 'NONE', #3662, .T. ) ;
#2179 = ORIENTED_EDGE ( 'NONE', *, *, #9491, .F. ) ;
#2180 = FACE_OUTER_BOUND ( 'NONE', #14430, .T. ) ;
#2181 = CIRCLE ( 'NONE', #22734, 0.7620000000000126672 ) ;
#2182 = PLANE ( 'NONE',  #12920 ) ;
#2183 = FACE_OUTER_BOUND ( 'NONE', #17695, .T. ) ;
#2184 = FACE_OUTER_BOUND ( 'NONE', #10767, .T. ) ;
#2185 = CARTESIAN_POINT ( 'NONE',  ( 18.09330115235438186, -3657.614207040705423, 2246.082635417008532 ) ) ;
#2186 = VERTEX_POINT ( 'NONE', #13680 ) ;
#2187 = CARTESIAN_POINT ( 'NONE',  ( 147.6247279057841411, -3695.594480551547804, 2259.836851275938898 ) ) ;
#2188 = DIRECTION ( 'NONE',  ( 1.000000000000000000, 0.000000000000000000, 0.000000000000000000 ) ) ;
#2189 =( BOUNDED_CURVE ( )  B_SPLINE_CURVE ( 3, ( #18273, #18158, #13117, #354 ),
 .UNSPECIFIED., .F., .T. ) 
 B_SPLINE_CURVE_WITH_KNOTS ( ( 4, 4 ),
 ( 1.570796327105885126, 3.141592653589766471 ),
 .UNSPECIFIED. ) 
 CURVE ( )  GEOMETRIC_REPRESENTATION_ITEM ( )  RATIONAL_B_SPLINE_CURVE ( ( 1.000000000000000000, 0.8047378541976719646, 0.8047378541976719646, 1.000000000000000000 ) ) 
 REPRESENTATION_ITEM ( '' )  );
#2190 = CARTESIAN_POINT ( 'NONE',  ( 3.810000000000000053, -3544.061999999999898, 2229.612000000000080 ) ) ;
#2191 = APPLIED_PERSON_AND_ORGANIZATION_ASSIGNMENT ( #4924, #6583, ( #20503 ) ) ;
#2192 = AXIS2_PLACEMENT_3D ( 'NONE', #15742, #5312, #10225 ) ;
#2193 = DIRECTION ( 'NONE',  ( -2.334777064352623371E-14, -1.000000000000000000, 0.000000000000000000 ) ) ;
#2194 = CARTESIAN_POINT ( 'NONE',  ( 142.0316867971391162, -3578.148799999964467, 2239.391000000000076 ) ) ;
#2195 = FACE_OUTER_BOUND ( 'NONE', #129, .T. ) ;
#2196 = CARTESIAN_POINT ( 'NONE',  ( 7.408172492505058493, -3577.337006982063031, 2244.988840501819595 ) ) ;
#2197 = ORIENTED_EDGE ( 'NONE', *, *, #9722, .T. ) ;
#2198 = APPROVAL_ROLE ( '' ) ;
#2199 = EDGE_CURVE ( 'NONE', #17590, #16242, #20830, .T. ) ;
#2200 = DIRECTION ( 'NONE',  ( 0.000000000000000000, 1.000000000000000000, 0.000000000000000000 ) ) ;
#2201 = DIRECTION ( 'NONE',  ( 0.000000000000000000, 0.000000000000000000, -1.000000000000000000 ) ) ;
#2202 = ADVANCED_FACE ( 'NONE', ( #11920 ), #19067, .F. ) ;
#2203 = DIRECTION ( 'NONE',  ( 0.000000000000000000, 0.000000000000000000, 1.000000000000000000 ) ) ;
#2204 = CARTESIAN_POINT ( 'NONE',  ( 134.6199999999999761, -3659.504999999999654, 2245.359999999999673 ) ) ;
#2205 = CARTESIAN_POINT ( 'NONE',  ( 124.1552000000010025, -3670.300000000000182, 2261.869999999999891 ) ) ;
#2206 = ORIENTED_EDGE ( 'NONE', *, *, #16409, .T. ) ;
#2207 = FACE_OUTER_BOUND ( 'NONE', #7045, .T. ) ;
#2208 = ORIENTED_EDGE ( 'NONE', *, *, #1697, .T. ) ;
#2209 = AXIS2_PLACEMENT_3D ( 'NONE', #14471, #2040, #3558 ) ;
#2210 = LINE ( 'NONE', #19905, #5083 ) ;
#2211 = CARTESIAN_POINT ( 'NONE',  ( 22.55520000000100111, -3670.300000000000182, 2261.869999999999891 ) ) ;
#2212 = ORIENTED_EDGE ( 'NONE', *, *, #19029, .F. ) ;
#2213 = DIRECTION ( 'NONE',  ( 0.000000000000000000, 1.000000000000000000, 0.000000000000000000 ) ) ;
#2214 = CARTESIAN_POINT ( 'NONE',  ( 14.05634339857000015, -3641.851755678999780, 2296.210799999999836 ) ) ;
#2215 = APPLIED_PERSON_AND_ORGANIZATION_ASSIGNMENT ( #3221, #1223, ( #18354 ) ) ;
#2216 = ORIENTED_EDGE ( 'NONE', *, *, #14685, .T. ) ;
#2217 = FACE_OUTER_BOUND ( 'NONE', #11646, .T. ) ;
#2218 = DIRECTION ( 'NONE',  ( 0.8660254037816071948, 0.5000000000049040771, 0.000000000000000000 ) ) ;
#2219 = ORIENTED_EDGE ( 'NONE', *, *, #11782, .T. ) ;
#2220 = EDGE_CURVE ( 'NONE', #8112, #7611, #3358, .T. ) ;
#2221 = FACE_OUTER_BOUND ( 'NONE', #7778, .T. ) ;
#2222 = ORIENTED_EDGE ( 'NONE', *, *, #20139, .T. ) ;
#2223 = CARTESIAN_POINT ( 'NONE',  ( 145.2268399904062051, -3580.949329744816623, 2245.461031122561053 ) ) ;
#2224 = ADVANCED_FACE ( 'NONE', ( #19421 ), #19532, .F. ) ;
#2225 = COORDINATED_UNIVERSAL_TIME_OFFSET ( 0, 0, .AHEAD. ) ;
#2226 = EDGE_CURVE ( 'NONE', #11524, #18611, #17893, .T. ) ;
#2227 = DIRECTION ( 'NONE',  ( 0.000000000000000000, 0.000000000000000000, -1.000000000000000000 ) ) ;
#2228 = DIRECTION ( 'NONE',  ( -0.6723379328345788775, -0.7402443542991228309, 0.000000000000000000 ) ) ;
#2229 = DIRECTION ( 'NONE',  ( 0.6887494619146010688, 0.000000000000000000, -0.7249994335945012525 ) ) ;
#2230 = CARTESIAN_POINT ( 'NONE',  ( 97.99320000000000164, -3670.300000000000182, 2239.771999999999935 ) ) ;
#2231 = DIRECTION ( 'NONE',  ( 0.000000000000000000, 1.000000000000000000, 0.000000000000000000 ) ) ;
#2232 = VERTEX_POINT ( 'NONE', #16134 ) ;
#2233 = CARTESIAN_POINT ( 'NONE',  ( 134.5048218173213854, -3577.113698916038629, 2245.146221591076028 ) ) ;
#2234 = ORIENTED_EDGE ( 'NONE', *, *, #13511, .T. ) ;
#2235 = SPHERICAL_SURFACE ( 'NONE', #3193, 0.7620000000000000107 ) ;
#2236 = VERTEX_POINT ( 'NONE', #1599 ) ;
#2237 = EDGE_CURVE ( 'NONE', #10346, #10620, #5379, .T. ) ;
#2238 = CARTESIAN_POINT ( 'NONE',  ( 10.68478392833999990, -3581.509597157999906, 2257.776259854999807 ) ) ;
#2239 =( GEOMETRIC_REPRESENTATION_CONTEXT ( 3 ) GLOBAL_UNCERTAINTY_ASSIGNED_CONTEXT ( ( #16504 ) ) GLOBAL_UNIT_ASSIGNED_CONTEXT ( ( #20317, #4258, #3913 ) ) REPRESENTATION_CONTEXT ( 'NONE', 'WORKASPACE' ) );
#2240 = CARTESIAN_POINT ( 'NONE',  ( 10.90494491371777208, -3657.298020409254605, 2247.542647217488138 ) ) ;
#2241 = ORIENTED_EDGE ( 'NONE', *, *, #182, .T. ) ;
#2242 = DIRECTION ( 'NONE',  ( 0.000000000000000000, 0.5000000000005969669, -0.8660254037840939834 ) ) ;
#2243 = CARTESIAN_POINT ( 'NONE',  ( 12.38520902594999917, -3596.664321836999989, 2279.814656244000162 ) ) ;
#2244 = ORIENTED_EDGE ( 'NONE', *, *, #13583, .T. ) ;
#2245 = DIRECTION ( 'NONE',  ( 0.000000000000000000, 0.000000000000000000, -1.000000000000000000 ) ) ;
#2246 = CARTESIAN_POINT ( 'NONE',  ( 15.20315289981203932, -3578.142343932459426, 2250.145168982875020 ) ) ;
#2247 = LINE ( 'NONE', #19947, #8695 ) ;
#2248 = EDGE_LOOP ( 'NONE', ( #14161, #15954, #19817, #5907 ) ) ;
#2249 = CARTESIAN_POINT ( 'NONE',  ( 10.21049783553369217, -3660.942314744965188, 2239.009999999927913 ) ) ;
#2250 = APPROVAL_ROLE ( '' ) ;
#2251 = AXIS2_PLACEMENT_3D ( 'NONE', #20840, #15569, #6552 ) ;
#2252 = ADVANCED_FACE ( 'NONE', ( #1839 ), #8985, .T. ) ;
#2253 = CARTESIAN_POINT ( 'NONE',  ( 12.69997737251000025, -3602.342301254000176, 2279.817638609000369 ) ) ;
#2254 = LINE ( 'NONE', #3891, #1201 ) ;
#2255 = VERTEX_POINT ( 'NONE', #7118 ) ;
#2256 = LOCAL_TIME ( 17, 37, 43.00000000000000000, #9170 ) ;
#2257 =( GEOMETRIC_REPRESENTATION_CONTEXT ( 3 ) GLOBAL_UNCERTAINTY_ASSIGNED_CONTEXT ( ( #16741 ) ) GLOBAL_UNIT_ASSIGNED_CONTEXT ( ( #21126, #3419, #23094 ) ) REPRESENTATION_CONTEXT ( 'NONE', 'WORKASPACE' ) );
#2258 = EDGE_CURVE ( 'NONE', #16093, #13523, #15074, .T. ) ;
#2259 = CARTESIAN_POINT ( 'NONE',  ( 136.8552000000009912, -3579.494999999999891, 2257.962944264955695 ) ) ;
#2260 = EDGE_CURVE ( 'NONE', #8915, #2597, #3592, .T. ) ;
#2261 = ORIENTED_EDGE ( 'NONE', *, *, #20057, .T. ) ;
#2262 = ORIENTED_EDGE ( 'NONE', *, *, #8594, .F. ) ;
#2263 = CARTESIAN_POINT ( 'NONE',  ( 141.1384052739540209, -3661.961130177203358, 2249.578382423867879 ) ) ;
#2264 = ORIENTED_EDGE ( 'NONE', *, *, #19899, .F. ) ;
#2265 = EDGE_CURVE ( 'NONE', #13234, #279, #18063, .T. ) ;
#2266 = ORIENTED_EDGE ( 'NONE', *, *, #12866, .F. ) ;
#2267 = VECTOR ( 'NONE', #21768, 1000.000000000000000 ) ;
#2268 = CARTESIAN_POINT ( 'NONE',  ( 9.903023377516998238, -3578.971306245000051, 2250.235372913999981 ) ) ;
#2269 = EDGE_LOOP ( 'NONE', ( #2708, #12650, #18630, #10324 ) ) ;
#2270 = APPROVAL_PERSON_ORGANIZATION ( #22012, #13928, #19919 ) ;
#2271 = DIRECTION ( 'NONE',  ( 0.000000000000000000, -1.000000000000000000, 0.000000000000000000 ) ) ;
#2272 = CARTESIAN_POINT ( 'NONE',  ( 151.1299999999999955, -3544.570000000000164, 2259.329999999999927 ) ) ;
#2273 = LOCAL_TIME ( 17, 37, 43.00000000000000000, #6917 ) ;
#2274 = EDGE_CURVE ( 'NONE', #12156, #11527, #121, .T. ) ;
#2275 = ORIENTED_EDGE ( 'NONE', *, *, #9441, .T. ) ;
#2276 = FACE_OUTER_BOUND ( 'NONE', #6897, .T. ) ;
#2277 = CARTESIAN_POINT ( 'NONE',  ( 29.00679999999900005, -3619.500000000000000, 2239.009999999999764 ) ) ;
#2278 = AXIS2_PLACEMENT_3D ( 'NONE', #10800, #7514, #5774 ) ;
#2279 = DIRECTION ( 'NONE',  ( -1.000000000000000000, 0.000000000000000000, 0.000000000000000000 ) ) ;
#2280 = DATE_AND_TIME ( #21954, #1522 ) ;
#2281 = EDGE_LOOP ( 'NONE', ( #2685, #16254, #18447, #22500 ) ) ;
#2282 = DIRECTION ( 'NONE',  ( -1.000000000000000000, -0.000000000000000000, -0.000000000000000000 ) ) ;
#2283 = ORIENTED_EDGE ( 'NONE', *, *, #19752, .T. ) ;
#2284 = CARTESIAN_POINT ( 'NONE',  ( 0.000000000000000000, -3660.140000000000327, 2243.277199999999993 ) ) ;
#2285 = ADVANCED_FACE ( 'NONE', ( #12275 ), #11204, .T. ) ;
#2286 = DIRECTION ( 'NONE',  ( -1.224646799147353207E-16, 1.000000000000000000, 0.000000000000000000 ) ) ;
#2287 = APPLIED_SECURITY_CLASSIFICATION_ASSIGNMENT ( #12016, ( #23169 ) ) ;
#2288 = APPLIED_APPROVAL_ASSIGNMENT ( #13489, ( #3469 ) ) ;
#2289 = ORIENTED_EDGE ( 'NONE', *, *, #2624, .T. ) ;
#2290 = DIRECTION ( 'NONE',  ( 1.000000000000000000, 0.000000000000000000, 0.000000000000000000 ) ) ;
#2291 = CARTESIAN_POINT ( 'NONE',  ( 12.69999999994000106, -3596.805100000000039, 2292.781800000000203 ) ) ;
#2292 = DIRECTION ( 'NONE',  ( 0.000000000000000000, 1.000000000000000000, 0.000000000000000000 ) ) ;
#2293 = DIRECTION ( 'NONE',  ( 0.000000000000000000, 2.336881798971000105E-14, 1.000000000000000000 ) ) ;
#2294 = AXIS2_PLACEMENT_3D ( 'NONE', #19270, #3205, #8606 ) ;
#2295 = CARTESIAN_POINT ( 'NONE',  ( 147.8270794805000037, -3543.299999999999727, 2259.329999999999927 ) ) ;
#2296 = EDGE_LOOP ( 'NONE', ( #15009, #19833, #11316, #19725 ) ) ;
#2297 = CARTESIAN_POINT ( 'NONE',  ( 34.49320000000000164, -3594.099999999999909, 2259.837999999999738 ) ) ;
#2298 = CARTESIAN_POINT ( 'NONE',  ( 139.6999999999999886, -3579.494999999999891, 2270.760000000000218 ) ) ;
#2299 = DIRECTION ( 'NONE',  ( 1.000000000000000000, 0.000000000000000000, 0.000000000000000000 ) ) ;
#2300 = EDGE_CURVE ( 'NONE', #10412, #16994, #3198, .T. ) ;
#2301 = LINE ( 'NONE', #6164, #9335 ) ;
#2302 = LINE ( 'NONE', #4504, #8714 ) ;
#2303 = LINE ( 'NONE', #8352, #7231 ) ;
#2304 = SECURITY_CLASSIFICATION ( '', '', #12352 ) ;
#2305 = LINE ( 'NONE', #5947, #9852 ) ;
#2306 = ORIENTED_EDGE ( 'NONE', *, *, #7142, .T. ) ;
#2307 = DATE_AND_TIME ( #18583, #396 ) ;
#2308 = ORIENTED_EDGE ( 'NONE', *, *, #12141, .T. ) ;
#2309 = LINE ( 'NONE', #2751, #10142 ) ;
#2310 = VECTOR ( 'NONE', #22317, 1000.000000000000000 ) ;
#2311 = AXIS2_PLACEMENT_3D ( 'NONE', #1538, #21240, #11971 ) ;
#2312 = CARTESIAN_POINT ( 'NONE',  ( 15.41268679715999923, -3657.938829547000296, 2239.009999999999764 ) ) ;
#2313 = LINE ( 'NONE', #11434, #1497 ) ;
#2314 = ORIENTED_EDGE ( 'NONE', *, *, #12075, .F. ) ;
#2315 = DIRECTION ( 'NONE',  ( 0.000000000000000000, -1.000000000000000000, 0.000000000000000000 ) ) ;
#2316 = APPLIED_PERSON_AND_ORGANIZATION_ASSIGNMENT ( #3949, #5495, ( #3396 ) ) ;
#2317 = FACE_OUTER_BOUND ( 'NONE', #8167, .T. ) ;
#2318 = VERTEX_POINT ( 'NONE', #7571 ) ;
#2319 =( BOUNDED_CURVE ( )  B_SPLINE_CURVE ( 3, ( #15784, #21297, #3005, #4879 ),
 .UNSPECIFIED., .F., .T. ) 
 B_SPLINE_CURVE_WITH_KNOTS ( ( 4, 4 ),
 ( -2.664535259100375697E-14, 1.570796326191299608 ),
 .UNSPECIFIED. ) 
 CURVE ( )  GEOMETRIC_REPRESENTATION_ITEM ( )  RATIONAL_B_SPLINE_CURVE ( ( 1.000000000000000000, 0.8047378542666279166, 0.8047378542666279166, 1.000000000000000000 ) ) 
 REPRESENTATION_ITEM ( '' )  );
#2320 = FACE_OUTER_BOUND ( 'NONE', #12713, .T. ) ;
#2321 = CARTESIAN_POINT ( 'NONE',  ( 139.6999999999999886, -3659.504999999999654, 2239.771999999999935 ) ) ;
#2322 = ORIENTED_EDGE ( 'NONE', *, *, #15440, .T. ) ;
#2323 = DIRECTION ( 'NONE',  ( 0.000000000000000000, 1.206582004152999850E-12, -1.000000000000000000 ) ) ;
#2324 = VECTOR ( 'NONE', #3075, 1000.000000000000000 ) ;
#2325 = CARTESIAN_POINT ( 'NONE',  ( 12.69999999999999929, -3659.504999999999654, 2270.760000000000218 ) ) ;
#2326 = AXIS2_PLACEMENT_3D ( 'NONE', #7377, #12647, #5514 ) ;
#2327 = ORIENTED_EDGE ( 'NONE', *, *, #20166, .T. ) ;
#2328 = DIRECTION ( 'NONE',  ( 0.000000000000000000, 1.000000000000000000, 1.224646799147353207E-16 ) ) ;
#2329 = DIRECTION ( 'NONE',  ( 0.000000000000000000, 0.000000000000000000, -1.000000000000000000 ) ) ;
#2330 = ORIENTED_EDGE ( 'NONE', *, *, #16011, .T. ) ;
#2331 = CARTESIAN_POINT ( 'NONE',  ( 137.1599999999999966, -3544.570000000000164, 2255.774000000000342 ) ) ;
#2332 = ORIENTED_EDGE ( 'NONE', *, *, #7003, .F. ) ;
#2333 = DIRECTION ( 'NONE',  ( 0.000000000000000000, -0.5000000000005969669, 0.8660254037840939834 ) ) ;
#2335 = CIRCLE ( 'NONE', #4565, 2.844799999998998796 ) ;
#2334 = APPROVAL_STATUS ( 'not_yet_approved' ) ;
#2336 = DIRECTION ( 'NONE',  ( 0.000000000000000000, 1.000000000000000000, 0.000000000000000000 ) ) ;
#2337 = CARTESIAN_POINT ( 'NONE',  ( 17.89998574415049504, -3661.876074222023362, 2245.138158857901090 ) ) ;
#2338 = TOROIDAL_SURFACE ( 'NONE', #9061, 4.114799999999999791, 1.270000000000000018 ) ;
#2339 = AXIS2_PLACEMENT_3D ( 'NONE', #17308, #1256, #15565 ) ;
#2340 = DIRECTION ( 'NONE',  ( 0.000000000000000000, 0.000000000000000000, -1.000000000000000000 ) ) ;
#2341 = PRODUCT_RELATED_PRODUCT_CATEGORY ( 'detail', '', ( #19099 ) ) ;
#2342 = CARTESIAN_POINT ( 'NONE',  ( 15.41268679715999923, -3577.928829547000078, 2239.009999999999764 ) ) ;
#2343 = AXIS2_PLACEMENT_3D ( 'NONE', #3245, #10157, #17412 ) ;
#2344 = CARTESIAN_POINT ( 'NONE',  ( 138.8064908466931229, -3576.792948563582740, 2249.346826069327562 ) ) ;
#2345 = B_SPLINE_CURVE_WITH_KNOTS ( 'NONE', 3,
 ( #6182, #16292, #19704, #131, #5405, #21455, #21799, #9033, #19930, #12661, #16940, #11138, #13320, #7163, #7934, #10903, #16179, #18277, #5761, #2121, #12894, #20052, #9382, #7275, #3987, #14547, #2233, #18051, #16826, #14312, #20470, #12547, #21683, #3869, #18161, #1880, #3745, #14426, #5642, #9151, #11017, #5532, #15082, #3634, #7395, #12775, #771, #4415, #21579, #11550, #2002, #10787 ),
 .UNSPECIFIED., .F., .F.,
 ( 4, 2, 1, 1, 1, 1, 2, 2, 2, 1, 2, 2, 2, 2, 1, 1, 1, 2, 2, 2, 2, 1, 1, 1, 2, 2, 2, 1, 1, 1, 2, 2, 4 ),
 ( 0.000000000000000000, 0.003906250000035784743, 0.007812500000071569486, 0.01562500000014313897, 0.03125000000029341807, 0.06250000000097141739, 0.1250000000023522018, 0.2500000000051094684, 0.2656250000053414495, 0.2812500000055733751, 0.3125000000065150108, 0.3750000000082734930, 0.5000000000120827792, 0.5019531250121850308, 0.5039062500122872823, 0.5078125000120770061, 0.5156250000117660326, 0.5312500000110412790, 0.5625000000099311670, 0.6250000000077041706, 0.6289062500076025852, 0.6328125000075008888, 0.6406250000076526563, 0.6562500000081283869, 0.6875000000090798480, 0.7500000000109762199, 0.7539062500107607256, 0.7578125000105452314, 0.7656250000102002851, 0.7812500000095102815, 0.8125000000080342399, 0.8750000000053581584, 1.000000000000000000 ),
 .UNSPECIFIED. ) ;
#2346 = EDGE_LOOP ( 'NONE', ( #7676, #13469, #20053, #4228 ) ) ;
#2347 = ADVANCED_FACE ( 'NONE', ( #4287, #2195 ), #22085, .F. ) ;
#2348 = VERTEX_POINT ( 'NONE', #2953 ) ;
#2349 = CARTESIAN_POINT ( 'NONE',  ( 12.69999999999999929, -3599.497499999999945, 2290.241799999999785 ) ) ;
#2350 = ORIENTED_EDGE ( 'NONE', *, *, #20870, .T. ) ;
#2351 = EDGE_CURVE ( 'NONE', #22988, #6254, #18464, .T. ) ;
#2352 = CARTESIAN_POINT ( 'NONE',  ( 13.63269713621999912, -3596.803664902999571, 2279.779803621000156 ) ) ;
#2353 = CARTESIAN_POINT ( 'NONE',  ( 140.0740604339752622, -3662.331215596936545, 2257.597438756872180 ) ) ;
#2354 = AXIS2_PLACEMENT_3D ( 'NONE', #1904, #21366, #3429 ) ;
#2355 = ADVANCED_FACE ( 'NONE', ( #16813 ), #9107, .T. ) ;
#2356 = VERTEX_POINT ( 'NONE', #11426 ) ;
#2357 = DIRECTION ( 'NONE',  ( 1.000000000000000000, 0.000000000000000000, 0.000000000000000000 ) ) ;
#2358 = DIRECTION ( 'NONE',  ( -1.000000000000000000, 0.000000000000000000, 0.000000000000000000 ) ) ;
#2359 = CIRCLE ( 'NONE', #18061, 5.080000000000000071 ) ;
#2360 = ORIENTED_EDGE ( 'NONE', *, *, #9679, .T. ) ;
#2361 = VECTOR ( 'NONE', #540, 1000.000000000000227 ) ;
#2362 = CARTESIAN_POINT ( 'NONE',  ( 10.36831320283000046, -3600.843699999999899, 2296.210799999999836 ) ) ;
#2363 = CARTESIAN_POINT ( 'NONE',  ( 14.01878970267436131, -3576.973962030261191, 2249.521889377991101 ) ) ;
#2364 = EDGE_CURVE ( 'NONE', #6776, #6888, #10586, .T. ) ;
#2365 = DIRECTION ( 'NONE',  ( -2.356218894535439317E-14, 0.000000000000000000, -1.000000000000000000 ) ) ;
#2366 = ORIENTED_EDGE ( 'NONE', *, *, #17387, .F. ) ;
#2367 = CARTESIAN_POINT ( 'NONE',  ( 19.17699999999900129, -3599.497499999999945, 2296.591799999999694 ) ) ;
#2368 = DATE_AND_TIME ( #20401, #16101 ) ;
#2369 = CARTESIAN_POINT ( 'NONE',  ( 136.9873132028999976, -3581.061170452877832, 2239.009999999999764 ) ) ;
#2370 = CARTESIAN_POINT ( 'NONE',  ( -12.70000000000008455, -3580.426170452909901, 2244.679313203224865 ) ) ;
#2371 = ORIENTED_EDGE ( 'NONE', *, *, #2952, .F. ) ;
#2372 = CARTESIAN_POINT ( 'NONE',  ( 67.10679999999999268, -3644.899999999999636, 2239.771999999999935 ) ) ;
#2373 = ADVANCED_FACE ( 'NONE', ( #18580 ), #22199, .T. ) ;
#2374 = ADVANCED_BREP_SHAPE_REPRESENTATION ( '', ( #21208, #5611 ), #14603 ) ;
#2375 = CIRCLE ( 'NONE', #18451, 3.606799999999993567 ) ;
#2376 = DIRECTION ( 'NONE',  ( 0.000000000000000000, -1.000000000000000000, 0.000000000000000000 ) ) ;
#2377 = ORIENTED_EDGE ( 'NONE', *, *, #14900, .T. ) ;
#2378 = AXIS2_PLACEMENT_3D ( 'NONE', #2392, #20318, #11291 ) ;
#2379 = CARTESIAN_POINT ( 'NONE',  ( 141.6834302667064662, -3661.544945296150217, 2249.865925870181400 ) ) ;
#2380 = AXIS2_PLACEMENT_3D ( 'NONE', #11967, #22619, #19118 ) ;
#2381 = EDGE_LOOP ( 'NONE', ( #22434, #18228, #18853, #7550, #7622, #543, #15958, #14647, #11502, #20253 ) ) ;
#2382 = EDGE_LOOP ( 'NONE', ( #3944, #2350 ) ) ;
#2383 = EDGE_CURVE ( 'NONE', #13491, #6446, #6849, .T. ) ;
#2384 = CARTESIAN_POINT ( 'NONE',  ( 15.18950216443630374, -3600.934814744946834, 2296.591800000036528 ) ) ;
#2385 = EDGE_LOOP ( 'NONE', ( #13367, #13612, #3782, #5739 ) ) ;
#2386 = DIRECTION ( 'NONE',  ( 1.000000000000000000, 0.000000000000000000, 0.000000000000000000 ) ) ;
#2387 = CARTESIAN_POINT ( 'NONE',  ( 12.69999999999999929, -3641.407499999999800, 2264.841800000000148 ) ) ;
#2388 = CIRCLE ( 'NONE', #6907, 1.270000000000000018 ) ;
#2389 = ORIENTED_EDGE ( 'NONE', *, *, #22609, .F. ) ;
#2390 = CARTESIAN_POINT ( 'NONE',  ( 7.146169398868164713, -3658.157008654403398, 2245.351788695067626 ) ) ;
#2391 = CARTESIAN_POINT ( 'NONE',  ( 15.03168679714000078, -3600.843699999999899, 2292.781800000000203 ) ) ;
#2392 = CARTESIAN_POINT ( 'NONE',  ( 151.1299999999999955, -3694.430000000000291, 2239.009999999999764 ) ) ;
#2393 = B_SPLINE_CURVE_WITH_KNOTS ( 'NONE', 3,
 ( #2573, #6333, #9721, #7971, #15119, #13467, #2240, #20608, #11941, #17442, #6797, #20727, #13940, #15461, #4554, #19212, #8555, #11825, #8198, #22717, #3267, #5034, #22477, #15345, #17206, #22593, #18981, #2922, #15697, #17323, #6448, #10299, #18856, #1393, #2798, #22938, #10414, #6688, #4796, #13589, #19330, #1152, #12058, #9944, #22826, #12179, #19093, #3150, #1271, #3033, #21088 ),
 .UNSPECIFIED., .F., .F.,
 ( 4, 2, 2, 2, 2, 1, 2, 2, 2, 2, 1, 1, 1, 2, 2, 2, 2, 2, 2, 1, 1, 2, 2, 2, 2, 1, 2, 2, 4 ),
 ( 0.000000000000000000, 0.1250000000061616823, 0.1875000000094276253, 0.2500000000126935684, 0.3125000000159595670, 0.3437500000176187398, 0.3593750000186234361, 0.3750000000196281325, 0.4375000000244468890, 0.4687500000268562395, 0.4843750000280609425, 0.4921875000287578295, 0.4960937500291060509, 0.4980468750292800784, 0.5000000000294539948, 0.5312500000300575120, 0.5625000000306610293, 0.5937500000312645465, 0.6093750000316296989, 0.6171875000318279847, 0.6210937500318399751, 0.6230468750317533777, 0.6250000000316668913, 0.6875000000274392731, 0.7187500000253340682, 0.7343750000242814657, 0.7421875000237551090, 0.7500000000232288633, 1.000000000000000000 ),
 .UNSPECIFIED. ) ;
#2394 = CARTESIAN_POINT ( 'NONE',  ( 116.8400000000000034, -3670.300000000000182, 2247.392000000000280 ) ) ;
#2395 = APPROVAL_ROLE ( '' ) ;
#2396 = FACE_OUTER_BOUND ( 'NONE', #5982, .T. ) ;
#2397 = CARTESIAN_POINT ( 'NONE',  ( 142.3526667532784415, -3658.477248352761308, 2249.700313726392324 ) ) ;
#2398 = CARTESIAN_POINT ( 'NONE',  ( 7.775933288980430014, -3662.408063519517327, 2245.667439000669219 ) ) ;
#2399 = ORIENTED_EDGE ( 'NONE', *, *, #9722, .F. ) ;
#2400 = AXIS2_PLACEMENT_3D ( 'NONE', #1495, #18132, #16490 ) ;
#2401 = DIRECTION ( 'NONE',  ( 0.000000000000000000, -1.000000000000000000, 0.000000000000000000 ) ) ;
#2402 = DIRECTION ( 'NONE',  ( 0.000000000000000000, -1.000000000000000000, 0.000000000000000000 ) ) ;
#2403 = ORIENTED_EDGE ( 'NONE', *, *, #12414, .T. ) ;
#2404 = DIRECTION ( 'NONE',  ( 0.000000000000000000, 0.000000000000000000, -1.000000000000000000 ) ) ;
#2405 = CARTESIAN_POINT ( 'NONE',  ( 18.25858294719762043, -3658.177107789667843, 2245.332874465672376 ) ) ;
#2406 = ORIENTED_EDGE ( 'NONE', *, *, #17721, .F. ) ;
#2407 = CARTESIAN_POINT ( 'NONE',  ( 145.1609999999999729, -3659.504999999999654, 2244.978999999999814 ) ) ;
#2408 = CARTESIAN_POINT ( 'NONE',  ( 139.6999999999999886, -3579.494999999999891, 2246.630000000000109 ) ) ;
#2409 = DIRECTION ( 'NONE',  ( 0.000000000000000000, -1.000000000000000000, 0.000000000000000000 ) ) ;
#2410 = ADVANCED_FACE ( 'NONE', ( #9339 ), #12086, .T. ) ;
#2411 = EDGE_CURVE ( 'NONE', #9808, #10881, #7979, .T. ) ;
#2412 = ADVANCED_FACE ( 'NONE', ( #12969 ), #20227, .T. ) ;
#2413 = DIRECTION ( 'NONE',  ( 0.000000000000000000, 0.000000000000000000, 1.000000000000000000 ) ) ;
#2414 = CARTESIAN_POINT ( 'NONE',  ( 10.36831320290272984, -3598.151299999887669, 2296.210799999999836 ) ) ;
#2415 = DIRECTION ( 'NONE',  ( 0.000000000000000000, -1.000000000000000000, 0.000000000000000000 ) ) ;
#2416 = EDGE_CURVE ( 'NONE', #18510, #16618, #10097, .T. ) ;
#2417 = CIRCLE ( 'NONE', #15504, 0.7619999999999294005 ) ;
#2418 = CARTESIAN_POINT ( 'NONE',  ( 7.619002919287616749, -3576.878850740295547, 2245.350237844942058 ) ) ;
#2419 = ORIENTED_EDGE ( 'NONE', *, *, #18994, .F. ) ;
#2420 = PERSON_AND_ORGANIZATION ( #5446, #1895 ) ;
#2421 = AXIS2_PLACEMENT_3D ( 'NONE', #14663, #11021, #9610 ) ;
#2422 = VECTOR ( 'NONE', #4283, 1000.000000000000000 ) ;
#2423 = DIRECTION ( 'NONE',  ( 0.000000000000000000, 1.000000000000000000, 0.000000000000000000 ) ) ;
#2424 = EDGE_CURVE ( 'NONE', #5311, #11834, #20766, .T. ) ;
#2425 = CARTESIAN_POINT ( 'NONE',  ( 9.856504185002760821, -3579.622864616615061, 2250.134322108942342 ) ) ;
#2426 = DIRECTION ( 'NONE',  ( 0.000000000000000000, 1.000000000000000000, 0.000000000000000000 ) ) ;
#2427 = VERTEX_POINT ( 'NONE', #1186 ) ;
#2428 = EDGE_CURVE ( 'NONE', #5562, #12269, #2303, .T. ) ;
#2429 = DIRECTION ( 'NONE',  ( 0.000000000000000000, 0.000000000000000000, 1.000000000000000000 ) ) ;
#2430 = EDGE_CURVE ( 'NONE', #7722, #13032, #9449, .T. ) ;
#2431 = VECTOR ( 'NONE', #5091, 1000.000000000000000 ) ;
#2432 = CARTESIAN_POINT ( 'NONE',  ( 38.10000000000000142, -3644.899999999999636, 2259.837999999999738 ) ) ;
#2433 = EDGE_LOOP ( 'NONE', ( #10818, #7057 ) ) ;
#2434 = VECTOR ( 'NONE', #1174, 1000.000000000000000 ) ;
#2435 = CARTESIAN_POINT ( 'NONE',  ( 13.69877355052640056, -3662.169030373610894, 2249.386253497014877 ) ) ;
#2436 = VECTOR ( 'NONE', #14637, 1000.000000000000000 ) ;
#2437 = CARTESIAN_POINT ( 'NONE',  ( 0.000000000000000000, -3544.061999999999898, 2253.487999999999829 ) ) ;
#2438 = VECTOR ( 'NONE', #9310, 1000.000000000000000 ) ;
#2439 = EDGE_LOOP ( 'NONE', ( #10885, #22374, #15745, #935, #2314, #21837, #11328, #19676, #5055, #7825, #11231, #11730 ) ) ;
#2440 = DIRECTION ( 'NONE',  ( 0.000000000000000000, 1.000000000000000000, 0.000000000000000000 ) ) ;
#2441 = DIRECTION ( 'NONE',  ( -0.8660254037820785955, -0.5000000000040877302, 3.192239903039919200E-14 ) ) ;
#2442 = ORIENTED_EDGE ( 'NONE', *, *, #4508, .T. ) ;
#2443 = DIRECTION ( 'NONE',  ( 1.000000000000000000, 0.000000000000000000, -2.336881798971000105E-14 ) ) ;
#2444 = FACE_OUTER_BOUND ( 'NONE', #14061, .T. ) ;
#2445 = VERTEX_POINT ( 'NONE', #5946 ) ;
#2446 = VERTEX_POINT ( 'NONE', #23092 ) ;
#2447 = FACE_OUTER_BOUND ( 'NONE', #301, .T. ) ;
#2448 = UNCERTAINTY_MEASURE_WITH_UNIT (LENGTH_MEASURE( 1.000000000000000082E-05 ), #7409, 'distance_accuracy_value', 'NONE');
#2449 = AXIS2_PLACEMENT_3D ( 'NONE', #1177, #6824, #17472 ) ;
#2450 = ORIENTED_EDGE ( 'NONE', *, *, #17383, .F. ) ;
#2451 = CARTESIAN_POINT ( 'NONE',  ( 12.69999999999999929, -3655.060000000000400, 2262.355140000000119 ) ) ;
#2452 = VECTOR ( 'NONE', #4908, 1000.000000000000000 ) ;
#2453 = PERSON_AND_ORGANIZATION_ROLE ( 'design_owner' ) ;
#2454 = AXIS2_PLACEMENT_3D ( 'NONE', #13206, #15090, #18600 ) ;
#2455 = AXIS2_PLACEMENT_3D ( 'NONE', #21588, #17937, #2133 ) ;
#2456 = CARTESIAN_POINT ( 'NONE',  ( 13.63269303062000048, -3642.196336588000122, 2279.779804022999997 ) ) ;
#2457 = CARTESIAN_POINT ( 'NONE',  ( 18.05792386179019360, -3661.493495574527515, 2244.888583955523700 ) ) ;
#2458 = AXIS2_PLACEMENT_3D ( 'NONE', #1173, #2704, #20409 ) ;
#2459 = CARTESIAN_POINT ( 'NONE',  ( 131.9679797520999784, -3544.321224513000288, 2260.577432830999896 ) ) ;
#2460 = LINE ( 'NONE', #14994, #12098 ) ;
#2461 = CARTESIAN_POINT ( 'NONE',  ( 137.6667760428054805, -3577.504318391805100, 2249.893487662036478 ) ) ;
#2462 = VERTEX_POINT ( 'NONE', #22629 ) ;
#2463 = CARTESIAN_POINT ( 'NONE',  ( -12.31899999999988005, -3660.140000000000327, 2252.472000000000207 ) ) ;
#2464 = DIRECTION ( 'NONE',  ( 0.000000000000000000, 0.000000000000000000, 1.000000000000000000 ) ) ;
#2465 = EDGE_LOOP ( 'NONE', ( #17999, #15347 ) ) ;
#2466 = VECTOR ( 'NONE', #17296, 1000.000000000000000 ) ;
#2467 = CARTESIAN_POINT ( 'NONE',  ( 123.3932000000010021, -3619.500000000000000, 2259.837999999999738 ) ) ;
#2468 = CARTESIAN_POINT ( 'NONE',  ( 142.4524393066650703, -3660.248099168110912, 2257.938841367611076 ) ) ;
#2469 = AXIS2_PLACEMENT_3D ( 'NONE', #7797, #6388, #8025 ) ;
#2470 = AXIS2_PLACEMENT_3D ( 'NONE', #12635, #21543, #14394 ) ;
#2471 = ORIENTED_EDGE ( 'NONE', *, *, #15609, .F. ) ;
#2472 = AXIS2_PLACEMENT_3D ( 'NONE', #1266, #12053, #7254 ) ;
#2473 = ORIENTED_EDGE ( 'NONE', *, *, #6301, .F. ) ;
#2474 = CARTESIAN_POINT ( 'NONE',  ( 12.69999999999999929, -3599.497499999999945, 2290.241799999999785 ) ) ;
#2475 = ORIENTED_EDGE ( 'NONE', *, *, #5543, .F. ) ;
#2476 = APPLIED_PERSON_AND_ORGANIZATION_ASSIGNMENT ( #10314, #10194, ( #6739 ) ) ;
#2477 = CARTESIAN_POINT ( 'NONE',  ( 20.34169023495000062, -3694.797466901999996, 2260.545675974999995 ) ) ;
#2478 = CARTESIAN_POINT ( 'NONE',  ( 14.85554178696724925, -3577.638356783953441, 2249.961210317602308 ) ) ;
#2479 = CIRCLE ( 'NONE', #4709, 0.3809999999999647002 ) ;
#2480 = CARTESIAN_POINT ( 'NONE',  ( 142.3168752137765409, -3580.610805610244370, 2249.634253063868982 ) ) ;
#2481 = ORIENTED_EDGE ( 'NONE', *, *, #5577, .T. ) ;
#2482 = PERSON_AND_ORGANIZATION_ROLE ( 'design_supplier' ) ;
#2483 = EDGE_CURVE ( 'NONE', #3518, #4940, #6607, .T. ) ;
#2484 = SPHERICAL_SURFACE ( 'NONE', #15627, 0.7620000000000000107 ) ;
#2485 = ORIENTED_EDGE ( 'NONE', *, *, #7515, .T. ) ;
#2487 = ADVANCED_FACE ( 'NONE', ( #11976, #19128, #12093, #13975, #5191 ), #13747, .T. ) ;
#2486 = DIRECTION ( 'NONE',  ( 0.000000000000000000, -1.000000000000000000, 0.000000000000000000 ) ) ;
#2488 = AXIS2_PLACEMENT_3D ( 'NONE', #21146, #1207, #13766 ) ;
#2489 = ADVANCED_FACE ( 'NONE', ( #13855 ), #14708, .T. ) ;
#2490 = LINE ( 'NONE', #22263, #21072 ) ;
#2491 = AXIS2_PLACEMENT_3D ( 'NONE', #5799, #7435, #14474 ) ;
#2492 = VERTEX_POINT ( 'NONE', #15964 ) ;
#2493 = CARTESIAN_POINT ( 'NONE',  ( -12.69999999998383977, -3580.297314745246695, 2249.881502164247649 ) ) ;
#2494 = VECTOR ( 'NONE', #8399, 1000.000000000000000 ) ;
#2495 = ORIENTED_EDGE ( 'NONE', *, *, #16030, .T. ) ;
#2496 = ORIENTED_EDGE ( 'NONE', *, *, #9066, .T. ) ;
#2497 = CARTESIAN_POINT ( 'NONE',  ( 1.270000000000000018, -3544.570000000000164, 2240.279999999999745 ) ) ;
#2498 = VERTEX_POINT ( 'NONE', #3067 ) ;
#2499 = CARTESIAN_POINT ( 'NONE',  ( 142.0316867971999955, -3580.841199999999844, 2239.391000000000076 ) ) ;
#2500 = DIRECTION ( 'NONE',  ( 0.000000000000000000, 0.000000000000000000, -1.000000000000000000 ) ) ;
#2501 = ORIENTED_EDGE ( 'NONE', *, *, #19684, .F. ) ;
#2502 = VECTOR ( 'NONE', #7547, 1000.000000000000000 ) ;
#2503 = CARTESIAN_POINT ( 'NONE',  ( 7.254080984692166112, -3657.771749848715444, 2245.815507489473475 ) ) ;
#2504 = CARTESIAN_POINT ( 'NONE',  ( 151.4000000000000057, -3544.061999999999898, 2280.589800000000196 ) ) ;
#2505 = DIRECTION ( 'NONE',  ( 0.7249994335945980639, 0.000000000000000000, 0.6887494619144990393 ) ) ;
#2506 = CARTESIAN_POINT ( 'NONE',  ( 12.70000000005999929, -3576.802599999999984, 2239.391000000000076 ) ) ;
#2507 = APPROVAL_ROLE ( '' ) ;
#2508 = ADVANCED_FACE ( 'NONE', ( #21005 ), #17708, .F. ) ;
#2509 = CYLINDRICAL_SURFACE ( 'NONE', #12038, 0.7619999999999294005 ) ;
#2510 = EDGE_CURVE ( 'NONE', #5555, #4126, #22550, .T. ) ;
#2511 = ADVANCED_FACE ( 'NONE', ( #19247 ), #12830, .T. ) ;
#2512 = CARTESIAN_POINT ( 'NONE',  ( 151.1299999999999955, -3660.140000000000327, 2247.392000000000280 ) ) ;
#2513 = DIRECTION ( 'NONE',  ( -1.000000000000000000, 0.000000000000000000, 0.000000000000000000 ) ) ;
#2514 = ORIENTED_EDGE ( 'NONE', *, *, #13583, .F. ) ;
#2515 = AXIS2_PLACEMENT_3D ( 'NONE', #16875, #9960, #821 ) ;
#2516 = LINE ( 'NONE', #5933, #8790 ) ;
#2517 = ORIENTED_EDGE ( 'NONE', *, *, #20569, .F. ) ;
#2518 = DIRECTION ( 'NONE',  ( -0.8660254037840939834, 0.5000000000005969669, 0.000000000000000000 ) ) ;
#2519 = FACE_OUTER_BOUND ( 'NONE', #15863, .T. ) ;
#2520 = CIRCLE ( 'NONE', #20856, 0.3810000000000002829 ) ;
#2521 = ORIENTED_EDGE ( 'NONE', *, *, #944, .F. ) ;
#2522 = ORIENTED_EDGE ( 'NONE', *, *, #9271, .T. ) ;
#2523 = DIRECTION ( 'NONE',  ( 1.000000000000000000, 0.000000000000000000, 0.000000000000000000 ) ) ;
#2524 = EDGE_CURVE ( 'NONE', #9946, #13188, #6949, .T. ) ;
#2525 = AXIS2_PLACEMENT_3D ( 'NONE', #10033, #773, #13550 ) ;
#2526 = DIRECTION ( 'NONE',  ( 1.122008997397786234E-13, 0.000000000000000000, 1.000000000000000000 ) ) ;
#2527 = CARTESIAN_POINT ( 'NONE',  ( 12.38525565295999975, -3602.330681407000156, 2279.814657614000225 ) ) ;
#2528 = DIRECTION ( 'NONE',  ( -1.000000000000000000, 1.206520773835000154E-12, 0.000000000000000000 ) ) ;
#2529 = FACE_OUTER_BOUND ( 'NONE', #12517, .T. ) ;
#2530 = DIRECTION ( 'NONE',  ( 1.000000000000000000, 0.000000000000000000, 0.000000000000000000 ) ) ;
#2531 = CARTESIAN_POINT ( 'NONE',  ( 20.53778376327932520, -3695.473260056960498, 2260.054522072026884 ) ) ;
#2532 = ORIENTED_EDGE ( 'NONE', *, *, #21399, .T. ) ;
#2533 = APPLICATION_PROTOCOL_DEFINITION ( 'international standard', 'automotive_design', 2000, #9618 ) ;
#2534 = CIRCLE ( 'NONE', #22730, 0.7619999999999294005 ) ;
#2535 = PLANE ( 'NONE',  #12774 ) ;
#2536 = VECTOR ( 'NONE', #522, 1000.000000000000000 ) ;
#2537 = CARTESIAN_POINT ( 'NONE',  ( 0.000000000000000000, -3543.299999999999727, 2275.001800000000003 ) ) ;
#2538 = FACE_OUTER_BOUND ( 'NONE', #15528, .T. ) ;
#2539 = ORIENTED_EDGE ( 'NONE', *, *, #402, .T. ) ;
#2540 = DIRECTION ( 'NONE',  ( 0.000000000000000000, 0.000000000000000000, -1.000000000000000000 ) ) ;
#2541 = EDGE_CURVE ( 'NONE', #5311, #1396, #22914, .T. ) ;
#2542 = EDGE_CURVE ( 'NONE', #1923, #9353, #2710, .T. ) ;
#2543 = CARTESIAN_POINT ( 'NONE',  ( 136.9873132028999976, -3581.061170452999704, 2239.009999999999764 ) ) ;
#2544 = ORIENTED_EDGE ( 'NONE', *, *, #3855, .T. ) ;
#2545 = CARTESIAN_POINT ( 'NONE',  ( 1.270000000000000018, -3695.699999999999818, 2240.279999999999745 ) ) ;
#2546 = DIRECTION ( 'NONE',  ( -2.343004830739999973E-14, -1.784212334590129905E-30, -1.000000000000000000 ) ) ;
#2547 = AXIS2_PLACEMENT_3D ( 'NONE', #19457, #3285, #21103 ) ;
#2548 = ORIENTED_EDGE ( 'NONE', *, *, #17718, .F. ) ;
#2549 = EDGE_CURVE ( 'NONE', #7810, #20367, #4529, .T. ) ;
#2550 = DIRECTION ( 'NONE',  ( 0.000000000000000000, 0.000000000000000000, -1.000000000000000000 ) ) ;
#2551 = CARTESIAN_POINT ( 'NONE',  ( 85.29320000000001301, -3644.899999999999636, 2260.600000000000364 ) ) ;
#2552 = DIRECTION ( 'NONE',  ( -1.000000000000000000, 0.000000000000000000, 0.000000000000000000 ) ) ;
#2553 = CARTESIAN_POINT ( 'NONE',  ( 144.3113860273000171, -3576.119152860999748, 2246.630000000000109 ) ) ;
#2554 = EDGE_CURVE ( 'NONE', #894, #12269, #4824, .T. ) ;
#2555 = ORIENTED_EDGE ( 'NONE', *, *, #21610, .F. ) ;
#2556 = EDGE_CURVE ( 'NONE', #20183, #5906, #4586, .T. ) ;
#2557 = CARTESIAN_POINT ( 'NONE',  ( 3.810000000000000053, -3694.938000000000102, 2229.612000000000080 ) ) ;
#2558 = ORIENTED_EDGE ( 'NONE', *, *, #9764, .F. ) ;
#2559 = CARTESIAN_POINT ( 'NONE',  ( 145.2825357078243940, -3580.718563226084370, 2245.237727082246693 ) ) ;
#2560 = DATE_AND_TIME ( #20836, #6401 ) ;
#2561 = DIRECTION ( 'NONE',  ( 0.000000000000000000, 0.000000000000000000, -1.000000000000000000 ) ) ;
#2562 = CARTESIAN_POINT ( 'NONE',  ( 17.74539221806004363, -3662.189252963443778, 2245.418801174103464 ) ) ;
#2563 = TOROIDAL_SURFACE ( 'NONE', #14556, 3.606799999998999695, 0.7620000000000000107 ) ;
#2564 = CARTESIAN_POINT ( 'NONE',  ( 127.0000000000000000, -3568.700000000000273, 2259.837999999999738 ) ) ;
#2565 = CARTESIAN_POINT ( 'NONE',  ( 10.32641459757000035, -3577.918429336999907, 2257.848701351999807 ) ) ;
#2566 = EDGE_CURVE ( 'NONE', #22942, #9004, #5736, .T. ) ;
#2567 = CARTESIAN_POINT ( 'NONE',  ( 137.1051927857304236, -3578.289462873045977, 2250.192425027783884 ) ) ;
#2568 = VERTEX_POINT ( 'NONE', #17833 ) ;
#2569 = DIRECTION ( 'NONE',  ( 0.000000000000000000, 0.000000000000000000, 1.000000000000000000 ) ) ;
#2570 = CARTESIAN_POINT ( 'NONE',  ( 139.6999999999999886, -3582.187399999999798, 2239.391000000000076 ) ) ;
#2571 = ORIENTED_EDGE ( 'NONE', *, *, #20905, .T. ) ;
#2572 = CARTESIAN_POINT ( 'NONE',  ( -12.31900000000000084, -3578.860000000000127, 2247.392000000000280 ) ) ;
#2573 = CARTESIAN_POINT ( 'NONE',  ( 10.78733304872000076, -3657.399152860999493, 2246.630000000000109 ) ) ;
#2574 = VERTEX_POINT ( 'NONE', #4947 ) ;
#2575 = ORIENTED_EDGE ( 'NONE', *, *, #23095, .F. ) ;
#2576 = ORIENTED_EDGE ( 'NONE', *, *, #18385, .T. ) ;
#2577 = CARTESIAN_POINT ( 'NONE',  ( 18.01287425286000143, -3581.600847139000052, 2246.630000000000109 ) ) ;
#2578 = CIRCLE ( 'NONE', #20535, 1.904999999999823501 ) ;
#2579 = EDGE_CURVE ( 'NONE', #12459, #7148, #1783, .T. ) ;
#2580 = ORIENTED_EDGE ( 'NONE', *, *, #5073, .T. ) ;
#2581 = DIRECTION ( 'NONE',  ( -3.101339145306999912E-14, -1.000000000000000000, -1.984857052996999759E-12 ) ) ;
#2582 = CARTESIAN_POINT ( 'NONE',  ( 13.82650316938843282, -3576.881401190747965, 2249.436478869484290 ) ) ;
#2583 = DIRECTION ( 'NONE',  ( 1.000000000000000000, 0.000000000000000000, 0.000000000000000000 ) ) ;
#2584 = CARTESIAN_POINT ( 'NONE',  ( 142.0561911310684877, -3581.089035798021541, 2249.159696853207151 ) ) ;
#2585 = ORIENTED_EDGE ( 'NONE', *, *, #15117, .F. ) ;
#2586 = DIRECTION ( 'NONE',  ( 0.000000000000000000, 0.000000000000000000, -1.000000000000000000 ) ) ;
#2587 = CALENDAR_DATE ( 2026, 26, 10 ) ;
#2588 = CARTESIAN_POINT ( 'NONE',  ( 12.69999999999999929, -3574.034000000000106, 2244.978999999999814 ) ) ;
#2589 = ORIENTED_EDGE ( 'NONE', *, *, #145, .F. ) ;
#2590 = DIRECTION ( 'NONE',  ( -1.224646799147353207E-16, 1.000000000000000000, 0.000000000000000000 ) ) ;
#2591 = CIRCLE ( 'NONE', #12333, 1.269999999999882334 ) ;
#2592 = CARTESIAN_POINT ( 'NONE',  ( 142.5448000000000093, -3579.494999999999891, 2256.063560000000052 ) ) ;
#2593 = VERTEX_POINT ( 'NONE', #22858 ) ;
#2594 = AXIS2_PLACEMENT_3D ( 'NONE', #21867, #5943, #656 ) ;
#2595 = LINE ( 'NONE', #4363, #22271 ) ;
#2596 = APPLIED_DATE_AND_TIME_ASSIGNMENT ( #901, #6201, ( #11243 ) ) ;
#2597 = VERTEX_POINT ( 'NONE', #3302 ) ;
#2598 = ORIENTED_EDGE ( 'NONE', *, *, #22441, .T. ) ;
#2599 = DIRECTION ( 'NONE',  ( 0.000000000000000000, 0.000000000000000000, -1.000000000000000000 ) ) ;
#2600 = ORIENTED_EDGE ( 'NONE', *, *, #17520, .T. ) ;
#2601 = LINE ( 'NONE', #20311, #10161 ) ;
#2602 = LINE ( 'NONE', #16558, #1301 ) ;
#2603 = CIRCLE ( 'NONE', #20214, 3.606800000000000228 ) ;
#2604 = ORIENTED_EDGE ( 'NONE', *, *, #14395, .T. ) ;
#2605 = CARTESIAN_POINT ( 'NONE',  ( 7.133249611714339800, -3658.211785038479775, 2245.300344505144039 ) ) ;
#2606 = CARTESIAN_POINT ( 'NONE',  ( 0.000000000000000000, 0.000000000000000000, 0.000000000000000000 ) ) ;
#2607 = FACE_OUTER_BOUND ( 'NONE', #17094, .T. ) ;
#2608 = PRODUCT_DEFINITION_FORMATION_WITH_SPECIFIED_SOURCE ( 'ANY', '', #12377, .NOT_KNOWN. ) ;
#2609 = CIRCLE ( 'NONE', #6035, 2.844799999999999773 ) ;
#2610 = LINE ( 'NONE', #16900, #19347 ) ;
#2611 = COORDINATED_UNIVERSAL_TIME_OFFSET ( 0, 0, .AHEAD. ) ;
#2612 = CARTESIAN_POINT ( 'NONE',  ( 85.29320000000001301, -3594.099999999999909, 2239.771999999999935 ) ) ;
#2613 = DIRECTION ( 'NONE',  ( 0.000000000000000000, 0.000000000000000000, -1.000000000000000000 ) ) ;
#2614 = DIRECTION ( 'NONE',  ( 0.000000000000000000, 0.000000000000000000, -1.000000000000000000 ) ) ;
#2615 = DIRECTION ( 'NONE',  ( 0.000000000000000000, 0.000000000000000000, -1.000000000000000000 ) ) ;
#2616 = VERTEX_POINT ( 'NONE', #10450 ) ;
#2617 = DIRECTION ( 'NONE',  ( 1.000000000000000000, 0.000000000000000000, 0.000000000000000000 ) ) ;
#2618 = VECTOR ( 'NONE', #5728, 1000.000000000000000 ) ;
#2619 = APPROVAL ( #7811, 'UNSPECIFIED' ) ;
#2620 = SECURITY_CLASSIFICATION ( '', '', #11681 ) ;
#2621 = EDGE_LOOP ( 'NONE', ( #9341, #4566, #18911, #14969 ) ) ;
#2622 = CARTESIAN_POINT ( 'NONE',  ( 142.1839422240020951, -3580.930228203060778, 2257.872821503999148 ) ) ;
#2623 = DIRECTION ( 'NONE',  ( 0.000000000000000000, 0.000000000000000000, -1.000000000000000000 ) ) ;
#2624 = EDGE_CURVE ( 'NONE', #14130, #16669, #6475, .T. ) ;
#2625 = ORIENTED_EDGE ( 'NONE', *, *, #17236, .F. ) ;
#2626 = ORIENTED_EDGE ( 'NONE', *, *, #10002, .T. ) ;
#2627 = DIRECTION ( 'NONE',  ( -2.318894227180156550E-14, -1.000000000000000000, 0.000000000000000000 ) ) ;
#2628 = EDGE_CURVE ( 'NONE', #12083, #15238, #6115, .T. ) ;
#2629 = CARTESIAN_POINT ( 'NONE',  ( 20.17309679555000201, -3694.556024844999683, 2260.454626673999883 ) ) ;
#2630 = CARTESIAN_POINT ( 'NONE',  ( 12.69999999999999929, -3579.494999999999891, 2239.009999999999764 ) ) ;
#2631 = EDGE_CURVE ( 'NONE', #15285, #12671, #1596, .T. ) ;
#2632 = DIRECTION ( 'NONE',  ( 0.000000000000000000, 0.000000000000000000, -1.000000000000000000 ) ) ;
#2633 = DIRECTION ( 'NONE',  ( 0.000000000000000000, 0.000000000000000000, 1.000000000000000000 ) ) ;
#2634 = DIRECTION ( 'NONE',  ( -1.000000000000000000, 0.000000000000000000, 0.000000000000000000 ) ) ;
#2635 = VERTEX_POINT ( 'NONE', #16417 ) ;
#2636 = PERSON_AND_ORGANIZATION_ROLE ( 'design_supplier' ) ;
#2637 = ORIENTED_EDGE ( 'NONE', *, *, #12280, .F. ) ;
#2638 = DIRECTION ( 'NONE',  ( 0.000000000000000000, 1.000000000000000000, 0.000000000000000000 ) ) ;
#2639 = LOCAL_TIME ( 17, 37, 43.00000000000000000, #19388 ) ;
#2640 = APPROVAL_PERSON_ORGANIZATION ( #7355, #17811, #21096 ) ;
#2641 = CARTESIAN_POINT ( 'NONE',  ( 19.05000000000000071, -3656.965000000000146, 2247.392000000000280 ) ) ;
#2642 = CARTESIAN_POINT ( 'NONE',  ( -8.890000000017000303, -3658.793800000000374, 2249.723686796999573 ) ) ;
#2643 = EDGE_CURVE ( 'NONE', #22051, #18291, #17688, .T. ) ;
#2644 = PERSON ( 'NAUO-PER11', 'UNSPECIFIED', 'UNSPECIFIED', ('UNSPECIFIED'), ('UNSPECIFIED'), ('UNSPECIFIED') ) ;
#2645 = VERTEX_POINT ( 'NONE', #17940 ) ;
#2646 = FACE_BOUND ( 'NONE', #5108, .T. ) ;
#2647 = AXIS2_PLACEMENT_3D ( 'NONE', #6740, #13880, #1447 ) ;
#2648 = CARTESIAN_POINT ( 'NONE',  ( 12.69999999999999929, -3599.497499999999945, 2264.841800000000148 ) ) ;
#2649 = DIRECTION ( 'NONE',  ( 0.000000000000000000, 0.000000000000000000, 1.000000000000000000 ) ) ;
#2650 = ORIENTED_EDGE ( 'NONE', *, *, #501, .F. ) ;
#2651 = DIRECTION ( 'NONE',  ( -1.000000000000000000, 0.000000000000000000, 0.000000000000000000 ) ) ;
#2652 = DIRECTION ( 'NONE',  ( 0.8660254037820102058, -0.5000000000042060799, 0.000000000000000000 ) ) ;
#2653 = ORIENTED_EDGE ( 'NONE', *, *, #4783, .F. ) ;
#2654 = DIRECTION ( 'NONE',  ( 0.000000000000000000, 1.000000000000000000, 0.000000000000000000 ) ) ;
#2655 = CARTESIAN_POINT ( 'NONE',  ( -6.349999999999999645, -3660.140000000000327, 2247.392000000000280 ) ) ;
#2656 = ADVANCED_FACE ( 'NONE', ( #16529 ), #4113, .T. ) ;
#2657 = DIRECTION ( 'NONE',  ( 0.000000000000000000, 0.000000000000000000, -1.000000000000000000 ) ) ;
#2658 = DIRECTION ( 'NONE',  ( -0.5000000000048030468, 0.8660254037816655925, 0.000000000000000000 ) ) ;
#2659 = EDGE_LOOP ( 'NONE', ( #15616, #9569, #19849, #1405 ) ) ;
#2660 = VECTOR ( 'NONE', #13310, 1000.000000000000000 ) ;
#2661 = ORIENTED_EDGE ( 'NONE', *, *, #16841, .F. ) ;
#2662 = EDGE_CURVE ( 'NONE', #12473, #13851, #5546, .T. ) ;
#2663 = CIRCLE ( 'NONE', #17637, 1.904999999999823501 ) ;
#2664 = EDGE_CURVE ( 'NONE', #22154, #19668, #13968, .T. ) ;
#2665 = CYLINDRICAL_SURFACE ( 'NONE', #12066, 11.11249999999985860 ) ;
#2666 = ORIENTED_EDGE ( 'NONE', *, *, #18028, .F. ) ;
#2667 = CARTESIAN_POINT ( 'NONE',  ( 145.1235917977560632, -3581.296656515026825, 2245.923799407241859 ) ) ;
#2668 = DATE_TIME_ROLE ( 'classification_date' ) ;
#2669 = CARTESIAN_POINT ( 'NONE',  ( 38.10000000000000142, -3594.099999999999909, 2259.837999999999738 ) ) ;
#2670 = CARTESIAN_POINT ( 'NONE',  ( 12.69999999999999929, -3639.502500000000055, 2290.241799999999785 ) ) ;
#2671 = DIRECTION ( 'NONE',  ( 1.000000000000000000, 0.000000000000000000, 0.000000000000000000 ) ) ;
#2672 = CYLINDRICAL_SURFACE ( 'NONE', #9830, 0.3810000000000330345 ) ;
#2673 = FACE_OUTER_BOUND ( 'NONE', #17168, .T. ) ;
#2674 = ORIENTED_EDGE ( 'NONE', *, *, #9713, .F. ) ;
#2675 = VECTOR ( 'NONE', #3797, 1000.000000000000000 ) ;
#2676 = EDGE_CURVE ( 'NONE', #19268, #2462, #7590, .T. ) ;
#2677 = FACE_OUTER_BOUND ( 'NONE', #6298, .T. ) ;
#2678 = VECTOR ( 'NONE', #4917, 1000.000000000000000 ) ;
#2679 = DIRECTION ( 'NONE',  ( 1.000000000000000000, -0.000000000000000000, 1.224646799147353207E-16 ) ) ;
#2680 = VERTEX_POINT ( 'NONE', #10799 ) ;
#2681 = DIRECTION ( 'NONE',  ( -1.000000000000000000, 0.000000000000000000, 0.000000000000000000 ) ) ;
#2682 = B_SPLINE_CURVE_WITH_KNOTS ( 'NONE', 3,
 ( #10336, #1431, #10099, #4826 ),
 .UNSPECIFIED., .F., .F.,
 ( 4, 4 ),
 ( 0.9999948892528710553, 1.000000000000000000 ),
 .UNSPECIFIED. ) ;
#2683 = CARTESIAN_POINT ( 'NONE',  ( 139.6999999999999886, -3570.287499999999909, 2268.705139999999574 ) ) ;
#2684 = VERTEX_POINT ( 'NONE', #18292 ) ;
#2685 = ORIENTED_EDGE ( 'NONE', *, *, #5585, .F. ) ;
#2686 = PERSON_AND_ORGANIZATION ( #14410, #18386 ) ;
#2687 = FACE_BOUND ( 'NONE', #455, .T. ) ;
#2688 = CIRCLE ( 'NONE', #97, 2.844800000000001550 ) ;
#2689 = EDGE_LOOP ( 'NONE', ( #21721, #1162, #10236, #6621, #22216 ) ) ;
#2690 = CARTESIAN_POINT ( 'NONE',  ( 12.69999999999999929, -3585.210000000000036, 2274.293139999999767 ) ) ;
#2691 = EDGE_CURVE ( 'NONE', #11827, #2024, #1890, .T. ) ;
#2692 = CARTESIAN_POINT ( 'NONE',  ( 11.02948398983750167, -3577.192243618181237, 2249.696728442258973 ) ) ;
#2693 = CARTESIAN_POINT ( 'NONE',  ( 142.3664352233508623, -3580.490377153994359, 2249.725648386253852 ) ) ;
#2694 = AXIS2_PLACEMENT_3D ( 'NONE', #9503, #19719, #17943 ) ;
#2695 = ORIENTED_EDGE ( 'NONE', *, *, #1052, .F. ) ;
#2697 = DIRECTION ( 'NONE',  ( 1.000000000000000000, 0.000000000000000000, 0.000000000000000000 ) ) ;
#2696 = AXIS2_PLACEMENT_3D ( 'NONE', #2145, #13037, #22462 ) ;
#2698 = APPLICATION_PROTOCOL_DEFINITION ( 'international standard', 'automotive_design', 2000, #12493 ) ;
#2699 = AXIS2_PLACEMENT_3D ( 'NONE', #9696, #7717, #16837 ) ;
#2700 = CARTESIAN_POINT ( 'NONE',  ( 7.619999999999999218, -3659.504999999999654, 2245.359999999999673 ) ) ;
#2701 = CARTESIAN_POINT ( 'NONE',  ( 20.37014473018363958, -3543.966768725831571, 2260.474410600547344 ) ) ;
#2702 = EDGE_CURVE ( 'NONE', #13348, #21028, #9467, .T. ) ;
#2703 = ORIENTED_EDGE ( 'NONE', *, *, #16004, .T. ) ;
#2704 = DIRECTION ( 'NONE',  ( 1.000000000000000000, 0.000000000000000000, 0.000000000000000000 ) ) ;
#2705 = ADVANCED_FACE ( 'NONE', ( #10914 ), #11258, .F. ) ;
#2706 = ADVANCED_FACE ( 'NONE', ( #9395 ), #12462, .T. ) ;
#2707 = ORIENTED_EDGE ( 'NONE', *, *, #2226, .F. ) ;
#2708 = ORIENTED_EDGE ( 'NONE', *, *, #5511, .F. ) ;
#2709 = AXIS2_PLACEMENT_3D ( 'NONE', #15787, #7686, #11203 ) ;
#2710 = CIRCLE ( 'NONE', #15824, 5.714999999999950120 ) ;
#2711 = DIRECTION ( 'NONE',  ( -0.000000000000000000, -1.000000000000000000, -0.000000000000000000 ) ) ;
#2712 = VERTEX_POINT ( 'NONE', #2135 ) ;
#2713 = FACE_OUTER_BOUND ( 'NONE', #13101, .T. ) ;
#2714 = CARTESIAN_POINT ( 'NONE',  ( 12.70000000000000107, -3589.528000000000247, 2275.817139999999654 ) ) ;
#2715 = ORIENTED_EDGE ( 'NONE', *, *, #1401, .F. ) ;
#2716 = CIRCLE ( 'NONE', #6482, 3.606799999999993567 ) ;
#2717 = CARTESIAN_POINT ( 'NONE',  ( 7.026240522554910051, -3658.819843006041538, 2244.872055837873631 ) ) ;
#2718 = DIRECTION ( 'NONE',  ( 0.000000000000000000, -1.000000000000000000, 0.000000000000000000 ) ) ;
#2719 = DIRECTION ( 'NONE',  ( 0.000000000000000000, 2.336881798971000105E-14, -1.000000000000000000 ) ) ;
#2720 = CIRCLE ( 'NONE', #6125, 1.269999999999882334 ) ;
#2721 = COORDINATED_UNIVERSAL_TIME_OFFSET ( 0, 0, .AHEAD. ) ;
#2722 = LINE ( 'NONE', #12103, #22508 ) ;
#2723 = DIRECTION ( 'NONE',  ( 1.000000000000000000, 0.000000000000000000, 0.000000000000000000 ) ) ;
#2724 = B_SPLINE_CURVE_WITH_KNOTS ( 'NONE', 3,
 ( #13679, #6423, #6543, #13562, #2774, #5889, #20171, #9917, #8060, #13442, #20582, #20701, #19189, #6892, #16020, #21300, #19420, #17770, #7117, #12152, #10393, #1726, #14034, #10624, #20944, #8531, #21186, #5243, #19306, #12035, #5361, #3472, #12500, #14157, #23037, #5010, #15907, #14267, #7012, #12384, #3356, #5131, #19531, #10507, #22916, #8876, #17532, #23146, #12274, #19650, #17892, #21412, #17648, #3591, #10274, #10746, #1598, #3124, #8759, #1838, #8984, #22691, #6663, #13800 ),
 .UNSPECIFIED., .F., .F.,
 ( 4, 2, 1, 1, 2, 2, 2, 2, 1, 2, 2, 2, 2, 1, 1, 2, 2, 2, 2, 1, 2, 2, 2, 2, 1, 2, 2, 2, 2, 2, 2, 2, 1, 2, 2, 4 ),
 ( 0.001021189648326963767, 0.06345736529341350352, 0.09467545311595677859, 0.1102844970271577435, 0.1180890189827582121, 0.1258935409383586945, 0.1883297165821066210, 0.2195478044041626053, 0.2351568483152942923, 0.2429613702709592371, 0.2507658922266241541, 0.3132020678728795748, 0.3444201556960073685, 0.3600291996077152334, 0.3678337215635693047, 0.3717359825415584296, 0.3756382435195474989, 0.4068563313439385043, 0.4224653752561136066, 0.4302698972122011578, 0.4341721581902011073, 0.4380744191682010014, 0.4692925069923846726, 0.4849015509043257399, 0.4927060728601833084, 0.4966083338381755974, 0.5005105948161677754, 0.5629467704654305127, 0.5941648582901043474, 0.6097739022023097588, 0.6253829461145151702, 0.6878191217629900933, 0.7190372095870988245, 0.7346462534990108040, 0.7502552974109228945, 1.000000000000000000 ),
 .UNSPECIFIED. ) ;
#2725 = AXIS2_PLACEMENT_3D ( 'NONE', #8586, #12095, #8474 ) ;
#2726 = CIRCLE ( 'NONE', #10229, 2.844799999999994444 ) ;
#2727 = DIRECTION ( 'NONE',  ( 1.000000000000000000, 0.000000000000000000, 0.000000000000000000 ) ) ;
#2728 = PLANE ( 'NONE',  #18624 ) ;
#2729 = EDGE_LOOP ( 'NONE', ( #18788, #2576 ) ) ;
#2730 = LINE ( 'NONE', #15396, #15971 ) ;
#2731 = ORIENTED_EDGE ( 'NONE', *, *, #16718, .T. ) ;
#2732 = ORIENTED_EDGE ( 'NONE', *, *, #211, .T. ) ;
#2733 = CIRCLE ( 'NONE', #2019, 2.844800000000091700 ) ;
#2734 = CARTESIAN_POINT ( 'NONE',  ( 136.8551999999999964, -3659.504999999999654, 2256.063560000000052 ) ) ;
#2735 = CARTESIAN_POINT ( 'NONE',  ( 144.7800000000000011, -3659.504999999999654, 2245.359999999999673 ) ) ;
#2736 = TOROIDAL_SURFACE ( 'NONE', #5762, 3.606799999999999784, 0.7620000000000000107 ) ;
#2737 = ORIENTED_EDGE ( 'NONE', *, *, #4275, .T. ) ;
#2738 = ORIENTED_EDGE ( 'NONE', *, *, #6251, .T. ) ;
#2739 = CARTESIAN_POINT ( 'NONE',  ( 12.69999999999999929, -3655.060000000000400, 2262.355140000000119 ) ) ;
#2740 = LINE ( 'NONE', #18795, #10256 ) ;
#2741 = LINE ( 'NONE', #9670, #17048 ) ;
#2742 = VECTOR ( 'NONE', #3932, 999.9999999999998863 ) ;
#2743 = DIRECTION ( 'NONE',  ( 0.000000000000000000, 1.000000000000000000, 0.000000000000000000 ) ) ;
#2744 = DIRECTION ( 'NONE',  ( 0.000000000000000000, 0.000000000000000000, -1.000000000000000000 ) ) ;
#2745 = DIRECTION ( 'NONE',  ( -1.000000000000000000, 0.000000000000000000, 0.000000000000000000 ) ) ;
#2746 = DIRECTION ( 'NONE',  ( -1.000000000000000000, 0.000000000000000000, 0.000000000000000000 ) ) ;
#2747 = ORIENTED_EDGE ( 'NONE', *, *, #14005, .F. ) ;
#2748 = APPROVAL_STATUS ( 'not_yet_approved' ) ;
#2749 = APPLIED_PERSON_AND_ORGANIZATION_ASSIGNMENT ( #8478, #15625, ( #17188 ) ) ;
#2750 = VERTEX_POINT ( 'NONE', #9163 ) ;
#2751 = CARTESIAN_POINT ( 'NONE',  ( 0.7620000000000000107, -3694.938000000000102, 2239.009999999999764 ) ) ;
#2752 = AXIS2_PLACEMENT_3D ( 'NONE', #20959, #7134, #1262 ) ;
#2753 = AXIS2_PLACEMENT_3D ( 'NONE', #7655, #2171, #11061 ) ;
#2754 = CARTESIAN_POINT ( 'NONE',  ( 9.901643740141382821, -3580.009520309946765, 2249.994425513007627 ) ) ;
#2755 = ADVANCED_FACE ( 'NONE', ( #12905 ), #18177, .T. ) ;
#2756 = CARTESIAN_POINT ( 'NONE',  ( 3.048000000000000043, -3544.061999999999898, 2238.248000000000047 ) ) ;
#2757 = ADVANCED_FACE ( 'NONE', ( #3882 ), #372, .T. ) ;
#2758 = VERTEX_POINT ( 'NONE', #14328 ) ;
#2759 = DIRECTION ( 'NONE',  ( 0.000000000000000000, 0.000000000000000000, 1.000000000000000000 ) ) ;
#2760 = EDGE_CURVE ( 'NONE', #3526, #7722, #18406, .T. ) ;
#2761 = FACE_OUTER_BOUND ( 'NONE', #22142, .T. ) ;
#2762 = CARTESIAN_POINT ( 'NONE',  ( 144.9135508633802942, -3661.845961013772467, 2245.115470801160882 ) ) ;
#2763 = ORIENTED_EDGE ( 'NONE', *, *, #2643, .F. ) ;
#2764 = DIRECTION ( 'NONE',  ( 0.000000000000000000, 0.000000000000000000, -1.000000000000000000 ) ) ;
#2765 = CARTESIAN_POINT ( 'NONE',  ( 14.37045735331549956, -3661.808175004912755, 2249.696654784097973 ) ) ;
#2766 = CARTESIAN_POINT ( 'NONE',  ( 137.3683132029000262, -3658.158799999999701, 2242.820000000000164 ) ) ;
#2767 = ORIENTED_EDGE ( 'NONE', *, *, #5212, .T. ) ;
#2768 = EDGE_CURVE ( 'NONE', #21577, #18508, #8503, .T. ) ;
#2769 = DIRECTION ( 'NONE',  ( 0.000000000000000000, -1.000000000000000000, 0.000000000000000000 ) ) ;
#2770 = VECTOR ( 'NONE', #7819, 1000.000000000000000 ) ;
#2771 = CARTESIAN_POINT ( 'NONE',  ( 13.92841025336000094, -3636.929928188000304, 2279.750815200000034 ) ) ;
#2772 = DIRECTION ( 'NONE',  ( 2.336881798971000105E-14, 2.336881798971000105E-14, 1.000000000000000000 ) ) ;
#2773 = AXIS2_PLACEMENT_3D ( 'NONE', #12728, #426, #7565 ) ;
#2774 = CARTESIAN_POINT ( 'NONE',  ( 15.51466946139100145, -3659.084409417217103, 2250.034617945921127 ) ) ;
#2775 = DIRECTION ( 'NONE',  ( 0.000000000000000000, 0.000000000000000000, -1.000000000000000000 ) ) ;
#2776 = EDGE_CURVE ( 'NONE', #19948, #2028, #13473, .T. ) ;
#2777 = VERTEX_POINT ( 'NONE', #11485 ) ;
#2778 = VERTEX_POINT ( 'NONE', #17103 ) ;
#2779 = CARTESIAN_POINT ( 'NONE',  ( -8.890000000022000748, -3580.206200000000081, 2245.060313203000078 ) ) ;
#2780 = VERTEX_POINT ( 'NONE', #2690 ) ;
#2781 = CARTESIAN_POINT ( 'NONE',  ( 140.0750197480601287, -3656.678786553412920, 2257.597441013359457 ) ) ;
#2782 = ITEM_DEFINED_TRANSFORMATION ( 'NONE', 'NONE', #21342,  #5611 ) ;
#2783 = CARTESIAN_POINT ( 'NONE',  ( 127.0000000000000000, -3670.300000000000182, 2261.869999999999891 ) ) ;
#2784 = DIRECTION ( 'NONE',  ( -1.000000000000000000, 0.000000000000000000, 0.000000000000000000 ) ) ;
#2785 = CARTESIAN_POINT ( 'NONE',  ( 17.73948428411033973, -3662.200341972358729, 2245.430382740787081 ) ) ;
#2786 = AXIS2_PLACEMENT_3D ( 'NONE', #16461, #21743, #21516 ) ;
#2787 = EDGE_CURVE ( 'NONE', #17996, #18205, #15241, .T. ) ;
#2788 = CARTESIAN_POINT ( 'NONE',  ( 12.69999999999999929, -3656.660200000000259, 2257.592639999999847 ) ) ;
#2789 = EDGE_CURVE ( 'NONE', #21067, #15388, #14128, .T. ) ;
#2790 = DIRECTION ( 'NONE',  ( 0.000000000000000000, 1.000000000000000000, 0.000000000000000000 ) ) ;
#2791 = CIRCLE ( 'NONE', #1287, 5.714999999999927915 ) ;
#2792 = CARTESIAN_POINT ( 'NONE',  ( 12.69999999999999929, -3590.289999999999964, 2268.705139999999574 ) ) ;
#2793 = ORIENTED_EDGE ( 'NONE', *, *, #14881, .T. ) ;
#2794 = CARTESIAN_POINT ( 'NONE',  ( 7.619999999999999218, -3659.504999999999654, 2239.391000000000076 ) ) ;
#2795 = CARTESIAN_POINT ( 'NONE',  ( 142.7470794804999912, -3543.299999999999727, 2254.503999999999905 ) ) ;
#2796 = ORIENTED_EDGE ( 'NONE', *, *, #8158, .T. ) ;
#2797 = DIRECTION ( 'NONE',  ( 0.000000000000000000, 1.000000000000000000, 0.000000000000000000 ) ) ;
#2798 = CARTESIAN_POINT ( 'NONE',  ( 10.30318750565348829, -3657.972703622658173, 2249.234803022183314 ) ) ;
#2799 = ORIENTED_EDGE ( 'NONE', *, *, #18836, .F. ) ;
#2800 = VERTEX_POINT ( 'NONE', #2477 ) ;
#2801 = ORIENTED_EDGE ( 'NONE', *, *, #14955, .F. ) ;
#2802 = CONTEXT_DEPENDENT_SHAPE_REPRESENTATION ( #2173, #12954 ) ;
#2803 = CARTESIAN_POINT ( 'NONE',  ( -12.69999999999997087, -3577.293829547214045, 2250.104686797002159 ) ) ;
#2804 = AXIS2_PLACEMENT_3D ( 'NONE', #14806, #4587, #619 ) ;
#2805 = AXIS2_PLACEMENT_3D ( 'NONE', #1824, #527, #13066 ) ;
#2806 = VERTEX_POINT ( 'NONE', #13363 ) ;
#2807 = AXIS2_PLACEMENT_3D ( 'NONE', #17091, #1151, #2797 ) ;
#2808 = DIRECTION ( 'NONE',  ( 0.000000000000000000, 0.000000000000000000, -1.000000000000000000 ) ) ;
#2809 = DIRECTION ( 'NONE',  ( 0.000000000000000000, 0.000000000000000000, 1.000000000000000000 ) ) ;
#2810 = CARTESIAN_POINT ( 'NONE',  ( 0.000000000000000000, 0.000000000000000000, 0.000000000000000000 ) ) ;
#2811 = AXIS2_PLACEMENT_3D ( 'NONE', #21696, #7285, #12784 ) ;
#2812 = CARTESIAN_POINT ( 'NONE',  ( 141.6290972793774188, -3581.586076845646858, 2248.209447196302335 ) ) ;
#2813 = EDGE_LOOP ( 'NONE', ( #17723, #20968, #17350, #19826 ) ) ;
#2814 = CARTESIAN_POINT ( 'NONE',  ( 138.2712681005278057, -3661.972087661942624, 2257.683753147038260 ) ) ;
#2815 = PERSON_AND_ORGANIZATION_ROLE ( 'design_owner' ) ;
#2816 = CARTESIAN_POINT ( 'NONE',  ( 10.16000000000000014, -3578.213872745999652, 2255.774000000000342 ) ) ;
#2817 = DIRECTION ( 'NONE',  ( 0.000000000000000000, 0.000000000000000000, 1.000000000000000000 ) ) ;
#2818 = CARTESIAN_POINT ( 'NONE',  ( 133.9885211612832734, -3659.275430740734464, 2244.678943280418480 ) ) ;
#2819 = AXIS2_PLACEMENT_3D ( 'NONE', #16498, #12992, #12554 ) ;
#2820 = ORIENTED_EDGE ( 'NONE', *, *, #9789, .F. ) ;
#2821 = CIRCLE ( 'NONE', #22638, 4.114799999999974034 ) ;
#2822 = CARTESIAN_POINT ( 'NONE',  ( -12.54218463272304085, -3580.206200000483932, 2249.723686796998663 ) ) ;
#2823 = EDGE_CURVE ( 'NONE', #12697, #2102, #8098, .T. ) ;
#2824 = EDGE_CURVE ( 'NONE', #16618, #7940, #22254, .T. ) ;
#2825 = AXIS2_PLACEMENT_3D ( 'NONE', #12406, #8659, #10640 ) ;
#2826 = VERTEX_POINT ( 'NONE', #9728 ) ;
#2827 = ADVANCED_FACE ( 'NONE', ( #7980 ), #2852, .T. ) ;
#2828 = ORIENTED_EDGE ( 'NONE', *, *, #3971, .F. ) ;
#2829 = DIRECTION ( 'NONE',  ( -2.848935406719999894E-12, 1.000000000000000000, 2.336881798978000141E-14 ) ) ;
#2830 = ORIENTED_EDGE ( 'NONE', *, *, #548, .F. ) ;
#2831 = VECTOR ( 'NONE', #15386, 1000.000000000000000 ) ;
#2832 = DIRECTION ( 'NONE',  ( -0.7249994335945011414, 0.000000000000000000, -0.6887494619146010688 ) ) ;
#2833 = DIRECTION ( 'NONE',  ( 0.000000000000000000, 0.000000000000000000, 1.000000000000000000 ) ) ;
#2834 = EDGE_CURVE ( 'NONE', #140, #21948, #18610, .T. ) ;
#2835 = ORIENTED_EDGE ( 'NONE', *, *, #15310, .F. ) ;
#2836 = CARTESIAN_POINT ( 'NONE',  ( 7.266527782489568210, -3657.733286618344209, 2245.875159459704719 ) ) ;
#2837 = CARTESIAN_POINT ( 'NONE',  ( 12.69999999999999929, -3581.400000000000091, 2270.760000000000218 ) ) ;
#2838 = AXIS2_PLACEMENT_3D ( 'NONE', #3323, #3210, #1450 ) ;
#2839 = AXIS2_PLACEMENT_3D ( 'NONE', #7371, #21886, #19907 ) ;
#2840 = DIRECTION ( 'NONE',  ( 1.000000000000000000, 0.000000000000000000, 0.000000000000000000 ) ) ;
#2841 = EDGE_CURVE ( 'NONE', #20865, #830, #7753, .T. ) ;
#2842 = PRODUCT_CONTEXT ( 'NONE', #7664, 'mechanical' ) ;
#2843 = VECTOR ( 'NONE', #21075, 1000.000000000000000 ) ;
#2844 = EDGE_CURVE ( 'NONE', #15557, #22556, #18987, .T. ) ;
#2845 = DIRECTION ( 'NONE',  ( 5.432398939370942693E-28, 1.000000000000000000, 2.336881798971000105E-14 ) ) ;
#2846 = DIRECTION ( 'NONE',  ( 1.224646799141920914E-16, -1.000000000000000000, -2.336881798971000421E-14 ) ) ;
#2847 = ORIENTED_EDGE ( 'NONE', *, *, #8379, .T. ) ;
#2848 = DIRECTION ( 'NONE',  ( 0.000000000000000000, 0.000000000000000000, 1.000000000000000000 ) ) ;
#2849 = CIRCLE ( 'NONE', #19321, 0.3809999999999647002 ) ;
#2850 = CARTESIAN_POINT ( 'NONE',  ( 35.56000000000000227, -3543.300000000000182, 2251.506800000000112 ) ) ;
#2851 = CARTESIAN_POINT ( 'NONE',  ( 0.7620000000000000107, -3543.299999999999727, 2239.771999999999935 ) ) ;
#2852 = TOROIDAL_SURFACE ( 'NONE', #14516, 3.606799999999999784, 0.7620000000000000107 ) ;
#2853 = AXIS2_PLACEMENT_3D ( 'NONE', #12374, #3461, #10614 ) ;
#2854 = ORIENTED_EDGE ( 'NONE', *, *, #23159, .T. ) ;
#2855 = DIRECTION ( 'NONE',  ( 0.000000000000000000, -1.000000000000000000, 0.000000000000000000 ) ) ;
#2856 = EDGE_CURVE ( 'NONE', #12473, #19963, #14905, .T. ) ;
#2857 = ORIENTED_EDGE ( 'NONE', *, *, #22697, .T. ) ;
#2858 = VERTEX_POINT ( 'NONE', #18635 ) ;
#2859 = DIRECTION ( 'NONE',  ( 0.000000000000000000, -0.5000000000002102762, 0.8660254037843172492 ) ) ;
#2860 = AXIS2_PLACEMENT_3D ( 'NONE', #7544, #5683, #9192 ) ;
#2861 = CARTESIAN_POINT ( 'NONE',  ( 18.37161333721848777, -3658.802287535873802, 2244.881330935113056 ) ) ;
#2862 = VERTEX_POINT ( 'NONE', #11368 ) ;
#2863 = ORIENTED_EDGE ( 'NONE', *, *, #22579, .T. ) ;
#2864 = FACE_OUTER_BOUND ( 'NONE', #9948, .T. ) ;
#2865 = DIRECTION ( 'NONE',  ( 1.000000000000000000, 0.000000000000000000, 0.000000000000000000 ) ) ;
#2866 = AXIS2_PLACEMENT_3D ( 'NONE', #15221, #20957, #22352 ) ;
#2867 = CIRCLE ( 'NONE', #5500, 6.477000000000010971 ) ;
#2868 = CARTESIAN_POINT ( 'NONE',  ( 9.855201422231997910, -3599.497499926000273, 2279.447341858000073 ) ) ;
#2869 = ORIENTED_EDGE ( 'NONE', *, *, #4706, .T. ) ;
#2870 = AXIS2_PLACEMENT_3D ( 'NONE', #12266, #19523, #5350 ) ;
#2871 = CARTESIAN_POINT ( 'NONE',  ( 9.855099624826999971, -3659.505002774999411, 2250.165042250000170 ) ) ;
#2872 = DIRECTION ( 'NONE',  ( 0.000000000000000000, 0.000000000000000000, -1.000000000000000000 ) ) ;
#2873 = FACE_OUTER_BOUND ( 'NONE', #3318, .T. ) ;
#2874 = CARTESIAN_POINT ( 'NONE',  ( 20.66917619022257924, -3695.636872341213348, 2259.725418502411685 ) ) ;
#2875 = ORIENTED_EDGE ( 'NONE', *, *, #2901, .T. ) ;
#2876 = PERSON_AND_ORGANIZATION ( #5446, #1895 ) ;
#2877 = APPLICATION_CONTEXT ( 'configuration controlled 3d designs of mechanical parts and assemblies' ) ;
#2878 = EDGE_LOOP ( 'NONE', ( #12663, #21022, #8564, #17436 ) ) ;
#2879 = DIRECTION ( 'NONE',  ( 0.000000000000000000, -1.000000000000000000, 0.000000000000000000 ) ) ;
#2880 = CIRCLE ( 'NONE', #15982, 7.111999999999785160 ) ;
#2881 = CARTESIAN_POINT ( 'NONE',  ( 10.84819624241226421, -3581.654767633020128, 2247.929782366414656 ) ) ;
#2882 = CIRCLE ( 'NONE', #5898, 0.7619999999999294005 ) ;
#2883 = CYLINDRICAL_SURFACE ( 'NONE', #13446, 5.460999999999938126 ) ;
#2884 = ORIENTED_EDGE ( 'NONE', *, *, #10419, .T. ) ;
#2885 = CARTESIAN_POINT ( 'NONE',  ( 95.25000000000000000, -3544.570000000000164, 2250.236800000000130 ) ) ;
#2886 = LINE ( 'NONE', #10030, #1284 ) ;
#2887 = CARTESIAN_POINT ( 'NONE',  ( 145.3776872988880768, -3660.157359719874876, 2244.547249493355139 ) ) ;
#2888 = VERTEX_POINT ( 'NONE', #15125 ) ;
#2889 = DIRECTION ( 'NONE',  ( -1.224646799147353207E-16, 1.000000000000000000, 0.000000000000000000 ) ) ;
#2890 = DIRECTION ( 'NONE',  ( 0.000000000000000000, -1.000000000000000000, 0.000000000000000000 ) ) ;
#2891 = APPROVAL ( #20744, 'UNSPECIFIED' ) ;
#2892 = EDGE_LOOP ( 'NONE', ( #8692, #7310, #275, #505 ) ) ;
#2893 = CARTESIAN_POINT ( 'NONE',  ( 15.03168679716000078, -3658.158799999999701, 2239.391000000000076 ) ) ;
#2894 = CARTESIAN_POINT ( 'NONE',  ( 12.70000000000000107, -3590.289999999999964, 2279.817639999999756 ) ) ;
#2895 = VECTOR ( 'NONE', #22037, 1000.000000000000000 ) ;
#2896 = EDGE_CURVE ( 'NONE', #1398, #12697, #7863, .T. ) ;
#2897 = DIRECTION ( 'NONE',  ( 0.000000000000000000, 0.000000000000000000, -1.000000000000000000 ) ) ;
#2898 = CARTESIAN_POINT ( 'NONE',  ( 10.12686798322000215, -3598.270251158000065, 2279.515935650000301 ) ) ;
#2899 = CARTESIAN_POINT ( 'NONE',  ( 12.69999999999999929, -3599.497499999999945, 2290.241799999999785 ) ) ;
#2900 = ORIENTED_EDGE ( 'NONE', *, *, #9181, .T. ) ;
#2901 = EDGE_CURVE ( 'NONE', #21361, #2318, #971, .T. ) ;
#2902 = VECTOR ( 'NONE', #19901, 1000.000000000000000 ) ;
#2903 = AXIS2_PLACEMENT_3D ( 'NONE', #11080, #14834, #20111 ) ;
#2904 = SPHERICAL_SURFACE ( 'NONE', #6798, 0.7620000000000000107 ) ;
#2905 = EDGE_LOOP ( 'NONE', ( #20352, #4001, #21345, #6760 ) ) ;
#2906 = CARTESIAN_POINT ( 'NONE',  ( 9.851243568427076269, -3543.401189131950559, 2255.000779105281708 ) ) ;
#2907 = COORDINATED_UNIVERSAL_TIME_OFFSET ( 0, 0, .AHEAD. ) ;
#2908 = CARTESIAN_POINT ( 'NONE',  ( 9.916854418464000176, -3578.905956564000007, 2250.236428761999832 ) ) ;
#2909 = CARTESIAN_POINT ( 'NONE',  ( 142.5262150965213550, -3579.120943345095384, 2257.957974173306866 ) ) ;
#2910 = CARTESIAN_POINT ( 'NONE',  ( 9.855200508393229697, -3659.504999998446692, 2257.962940200992307 ) ) ;
#2911 = DIRECTION ( 'NONE',  ( 0.000000000000000000, 0.000000000000000000, -1.000000000000000000 ) ) ;
#2912 = CARTESIAN_POINT ( 'NONE',  ( 127.0000000000000000, -3670.300000000000182, 2259.837999999999738 ) ) ;
#2913 = VECTOR ( 'NONE', #11235, 1000.000000000000000 ) ;
#2914 = CARTESIAN_POINT ( 'NONE',  ( 137.4507161353425886, -3577.751214325344790, 2250.012832018660902 ) ) ;
#2915 = VERTEX_POINT ( 'NONE', #20505 ) ;
#2916 = CARTESIAN_POINT ( 'NONE',  ( 28.24479999999899604, -3568.700000000000273, 2239.771999999999935 ) ) ;
#2917 = AXIS2_PLACEMENT_3D ( 'NONE', #14073, #16057, #10898 ) ;
#2918 = APPLIED_DATE_AND_TIME_ASSIGNMENT ( #4750, #8507, ( #6775 ) ) ;
#2919 = CARTESIAN_POINT ( 'NONE',  ( 12.69999999999999929, -3639.502500000000055, 2290.241799999999785 ) ) ;
#2920 = EDGE_LOOP ( 'NONE', ( #23069, #22694, #15755, #16947 ) ) ;
#2921 = LINE ( 'NONE', #9943, #15921 ) ;
#2922 = CARTESIAN_POINT ( 'NONE',  ( 10.49306405180820612, -3657.709384941907501, 2248.871247615949414 ) ) ;
#2923 = ORIENTED_EDGE ( 'NONE', *, *, #13534, .T. ) ;
#2924 = EDGE_CURVE ( 'NONE', #9308, #12115, #4684, .T. ) ;
#2925 = ORIENTED_EDGE ( 'NONE', *, *, #9144, .T. ) ;
#2926 = CARTESIAN_POINT ( 'NONE',  ( 134.3066495004684668, -3581.385628414011080, 2246.082317947095362 ) ) ;
#2927 = PRODUCT_DEFINITION_CONTEXT ( 'detailed design', #7699, 'design' ) ;
#2928 = VERTEX_POINT ( 'NONE', #9619 ) ;
#2929 = EDGE_CURVE ( 'NONE', #19560, #20662, #244, .T. ) ;
#2930 = CIRCLE ( 'NONE', #5183, 1.269999999999882334 ) ;
#2931 = DIRECTION ( 'NONE',  ( -0.7071067811865969777, 0.000000000000000000, 0.7071067811864980568 ) ) ;
#2932 = DIRECTION ( 'NONE',  ( 0.000000000000000000, 1.000000000000000000, 0.000000000000000000 ) ) ;
#2933 = DIRECTION ( 'NONE',  ( 0.000000000000000000, 0.000000000000000000, 1.000000000000000000 ) ) ;
#2934 = CARTESIAN_POINT ( 'NONE',  ( 142.2663395169348064, -3580.722924689276624, 2249.542540277683202 ) ) ;
#2935 = EDGE_LOOP ( 'NONE', ( #10604, #9279, #17265, #22529 ) ) ;
#2936 = CARTESIAN_POINT ( 'NONE',  ( 138.9568795186264936, -3582.247434258886642, 2257.615983644609059 ) ) ;
#2937 = COORDINATED_UNIVERSAL_TIME_OFFSET ( 0, 0, .AHEAD. ) ;
#2938 = DIRECTION ( 'NONE',  ( -2.580078660703000173E-14, 2.590196616235000036E-13, -1.000000000000000000 ) ) ;
#2939 = CARTESIAN_POINT ( 'NONE',  ( 14.64973061487417816, -3581.566609002860787, 2248.268300351840935 ) ) ;
#2940 = PLANE ( 'NONE',  #846 ) ;
#2941 = EDGE_CURVE ( 'NONE', #17865, #12626, #11591, .T. ) ;
#2942 = ORIENTED_EDGE ( 'NONE', *, *, #21990, .F. ) ;
#2943 = DIRECTION ( 'NONE',  ( 0.000000000000000000, -1.000000000000000000, 0.000000000000000000 ) ) ;
#2944 = DIRECTION ( 'NONE',  ( -2.848812946084999742E-12, -1.000000000000000000, 0.000000000000000000 ) ) ;
#2945 = ORIENTED_EDGE ( 'NONE', *, *, #7414, .F. ) ;
#2946 = TOROIDAL_SURFACE ( 'NONE', #2209, 3.606799999998999695, 0.7620000000000000107 ) ;
#2947 = DIRECTION ( 'NONE',  ( 0.000000000000000000, 0.000000000000000000, 1.000000000000000000 ) ) ;
#2948 = CARTESIAN_POINT ( 'NONE',  ( -5.588000000000000078, -3578.860000000000127, 2250.236800000000130 ) ) ;
#2949 = EDGE_LOOP ( 'NONE', ( #14778, #12228 ) ) ;
#2950 = DIRECTION ( 'NONE',  ( -0.000000000000000000, 1.000000000000000000, 0.000000000000000000 ) ) ;
#2951 = ORIENTED_EDGE ( 'NONE', *, *, #13866, .T. ) ;
#2952 = EDGE_CURVE ( 'NONE', #2498, #12177, #710, .T. ) ;
#2953 = CARTESIAN_POINT ( 'NONE',  ( 137.3683132029000262, -3658.158799999999701, 2242.820000000000164 ) ) ;
#2954 = CARTESIAN_POINT ( 'NONE',  ( 15.49256139849371117, -3660.048737986045126, 2250.235547086222141 ) ) ;
#2955 = DIRECTION ( 'NONE',  ( 0.000000000000000000, 0.000000000000000000, -1.000000000000000000 ) ) ;
#2956 = LINE ( 'NONE', #10102, #11863 ) ;
#2957 = PERSON_AND_ORGANIZATION ( #5446, #1895 ) ;
#2958 = EDGE_CURVE ( 'NONE', #17137, #13472, #9222, .T. ) ;
#2959 = ADVANCED_FACE ( 'NONE', ( #21217 ), #22292, .T. ) ;
#2960 = CYLINDRICAL_SURFACE ( 'NONE', #18180, 1.269999999999882334 ) ;
#2961 = DIRECTION ( 'NONE',  ( -1.000000000000000000, 0.000000000000000000, 0.000000000000000000 ) ) ;
#2962 = CARTESIAN_POINT ( 'NONE',  ( 64.76999999999999602, -3543.299999999999727, 2292.819899999999961 ) ) ;
#2963 = AXIS2_PLACEMENT_3D ( 'NONE', #5360, #3819, #14156 ) ;
#2964 = LINE ( 'NONE', #20776, #12455 ) ;
#2965 = EDGE_CURVE ( 'NONE', #10895, #22243, #13326, .T. ) ;
#2966 = VERTEX_POINT ( 'NONE', #6575 ) ;
#2967 = CARTESIAN_POINT ( 'NONE',  ( 137.1293827860164640, -3544.133557167025174, 2255.697297437880934 ) ) ;
#2968 = ORIENTED_EDGE ( 'NONE', *, *, #17310, .F. ) ;
#2969 = EDGE_CURVE ( 'NONE', #18582, #5364, #22725, .T. ) ;
#2970 = CARTESIAN_POINT ( 'NONE',  ( 4.657535968477718669, -3695.684982101911828, 2259.542693485130258 ) ) ;
#2971 = CARTESIAN_POINT ( 'NONE',  ( 22.54063073453000143, -3543.299999999999727, 2275.763800000000174 ) ) ;
#2972 = VERTEX_POINT ( 'NONE', #4919 ) ;
#2973 = ORIENTED_EDGE ( 'NONE', *, *, #13090, .F. ) ;
#2974 = APPROVAL_PERSON_ORGANIZATION ( #17511, #5791, #4628 ) ;
#2975 = CARTESIAN_POINT ( 'NONE',  ( -6.349999999999999645, -3694.938000000000102, 2253.487999999999829 ) ) ;
#2976 = DIRECTION ( 'NONE',  ( 0.000000000000000000, 0.000000000000000000, 1.000000000000000000 ) ) ;
#2977 = AXIS2_PLACEMENT_3D ( 'NONE', #8380, #12121, #15522 ) ;
#2978 = DIRECTION ( 'NONE',  ( 0.000000000000000000, 1.000000000000000000, 0.000000000000000000 ) ) ;
#2979 = EDGE_LOOP ( 'NONE', ( #21611, #7007, #21369, #11499 ) ) ;
#2980 = DIRECTION ( 'NONE',  ( -2.324635735433000053E-14, 0.000000000000000000, -1.000000000000000000 ) ) ;
#2981 = CARTESIAN_POINT ( 'NONE',  ( 124.1552000000010025, -3670.300000000000182, 2239.771999999999935 ) ) ;
#2982 = CYLINDRICAL_SURFACE ( 'NONE', #20340, 0.7619999999999996776 ) ;
#2983 = DIRECTION ( 'NONE',  ( 0.000000000000000000, 0.000000000000000000, 1.000000000000000000 ) ) ;
#2984 = CARTESIAN_POINT ( 'NONE',  ( 20.52304216182480445, -3695.446428763979839, 2260.091482594895751 ) ) ;
#2985 = EDGE_LOOP ( 'NONE', ( #23150, #7018, #9034, #15531 ) ) ;
#2986 = PERSON_AND_ORGANIZATION_ROLE ( 'design_owner' ) ;
#2987 = EDGE_CURVE ( 'NONE', #13032, #6140, #19100, .T. ) ;
#2988 = ORIENTED_EDGE ( 'NONE', *, *, #7501, .T. ) ;
#2989 = DIRECTION ( 'NONE',  ( 0.000000000000000000, -1.000000000000000000, 0.000000000000000000 ) ) ;
#2990 = CIRCLE ( 'NONE', #4843, 0.7619999999999294005 ) ;
#2991 = CARTESIAN_POINT ( 'NONE',  ( 10.78723565514999905, -3581.600816721000228, 2246.630000000000109 ) ) ;
#2992 = DIRECTION ( 'NONE',  ( 0.000000000000000000, 0.000000000000000000, -1.000000000000000000 ) ) ;
#2993 = LOCAL_TIME ( 17, 37, 43.00000000000000000, #5658 ) ;
#2994 = AXIS2_PLACEMENT_3D ( 'NONE', #9730, #20618, #20507 ) ;
#2995 = ORIENTED_EDGE ( 'NONE', *, *, #13453, .T. ) ;
#2996 = DIRECTION ( 'NONE',  ( 0.000000000000000000, -1.000000000000000000, 0.000000000000000000 ) ) ;
#2997 = CARTESIAN_POINT ( 'NONE',  ( 14.05634339859000015, -3657.155744320999929, 2239.391000000000076 ) ) ;
#2998 = CARTESIAN_POINT ( 'NONE',  ( 145.3283279854914554, -3660.498787106118925, 2244.568960851285283 ) ) ;
#2999 = PLANE ( 'NONE',  #14483 ) ;
#3000 = EDGE_CURVE ( 'NONE', #7148, #2806, #18196, .T. ) ;
#3001 = CARTESIAN_POINT ( 'NONE',  ( 10.97468688268398651, -3661.767038422824953, 2249.725556830857840 ) ) ;
#3002 = PRODUCT_DEFINITION_SHAPE ( 'NONE', 'NONE',  #12786 ) ;
#3003 = CARTESIAN_POINT ( 'NONE',  ( 147.4094809636181651, -3543.848287272899142, 2260.375776696899720 ) ) ;
#3004 = ORIENTED_EDGE ( 'NONE', *, *, #19432, .T. ) ;
#3005 = CARTESIAN_POINT ( 'NONE',  ( 137.2104978357572236, -3578.057685255099841, 2239.010000000134823 ) ) ;
#3006 = CARTESIAN_POINT ( 'NONE',  ( 47.19319999999999737, -3619.500000000000000, 2260.600000000000364 ) ) ;
#3007 = DIRECTION ( 'NONE',  ( 2.150065550568999996E-13, 0.000000000000000000, -1.000000000000000000 ) ) ;
#3008 = CARTESIAN_POINT ( 'NONE',  ( 12.69999999999999929, -3576.320000000000164, 2270.760000000000218 ) ) ;
#3009 = DIRECTION ( 'NONE',  ( -1.000000000000000000, 0.000000000000000000, 0.000000000000000000 ) ) ;
#3010 = APPLIED_APPROVAL_ASSIGNMENT ( #17344, ( #22928 ) ) ;
#3011 = ORIENTED_EDGE ( 'NONE', *, *, #404, .T. ) ;
#3012 = APPROVAL_PERSON_ORGANIZATION ( #11265, #6342, #2250 ) ;
#3013 = ORIENTED_EDGE ( 'NONE', *, *, #16965, .F. ) ;
#3014 = DIRECTION ( 'NONE',  ( -0.000000000000000000, -1.000000000000000000, -0.000000000000000000 ) ) ;
#3015 = EDGE_LOOP ( 'NONE', ( #14055, #14205, #21740, #14609 ) ) ;
#3016 = CARTESIAN_POINT ( 'NONE',  ( 139.6999999999999886, -3659.504999999999654, 2245.359999999999673 ) ) ;
#3017 = APPROVAL_STATUS ( 'not_yet_approved' ) ;
#3018 = PRODUCT_RELATED_PRODUCT_CATEGORY ( 'detail', '', ( #16881 ) ) ;
#3019 = DIRECTION ( 'NONE',  ( -1.000000000000000000, 0.000000000000000000, 0.000000000000000000 ) ) ;
#3020 = EDGE_LOOP ( 'NONE', ( #13992, #2580, #9940, #621 ) ) ;
#3021 = CARTESIAN_POINT ( 'NONE',  ( 142.5447999999989861, -3579.494999999999891, 2272.030000000000200 ) ) ;
#3022 = CARTESIAN_POINT ( 'NONE',  ( 40.94480000000000075, -3644.899999999999636, 2259.837999999999738 ) ) ;
#3023 = LINE ( 'NONE', #22707, #5139 ) ;
#3024 = FACE_OUTER_BOUND ( 'NONE', #2030, .T. ) ;
#3025 = APPLIED_APPROVAL_ASSIGNMENT ( #20631, ( #16852 ) ) ;
#3026 = DIRECTION ( 'NONE',  ( 0.000000000000000000, 0.000000000000000000, -1.000000000000000000 ) ) ;
#3027 = ORIENTED_EDGE ( 'NONE', *, *, #14685, .F. ) ;
#3028 = APPROVAL_PERSON_ORGANIZATION ( #11620, #18949, #19135 ) ;
#3029 = CARTESIAN_POINT ( 'NONE',  ( 50.79999999999999716, -3568.700000000000273, 2261.869999999999891 ) ) ;
#3030 = DIRECTION ( 'NONE',  ( -1.000000000000000000, 0.000000000000000000, 0.000000000000000000 ) ) ;
#3031 = ORIENTED_EDGE ( 'NONE', *, *, #22869, .F. ) ;
#3032 = CARTESIAN_POINT ( 'NONE',  ( 10.16000000000000014, -3660.786127253999894, 2255.774000000000342 ) ) ;
#3033 = CARTESIAN_POINT ( 'NONE',  ( 9.855099624826999971, -3659.161788968266592, 2250.086432307065934 ) ) ;
#3034 = CIRCLE ( 'NONE', #1921, 0.7619999999999987894 ) ;
#3035 = EDGE_LOOP ( 'NONE', ( #18348, #22438 ) ) ;
#3036 = CIRCLE ( 'NONE', #8649, 5.460999999999938126 ) ;
#3037 = VERTEX_POINT ( 'NONE', #19221 ) ;
#3038 = ORIENTED_EDGE ( 'NONE', *, *, #434, .F. ) ;
#3039 = DIRECTION ( 'NONE',  ( 0.000000000000000000, 0.000000000000000000, -1.000000000000000000 ) ) ;
#3040 = DIRECTION ( 'NONE',  ( 1.000000000000000000, 0.000000000000000000, 0.000000000000000000 ) ) ;
#3041 = DIRECTION ( 'NONE',  ( 0.000000000000000000, 0.000000000000000000, -1.000000000000000000 ) ) ;
#3042 = ORIENTED_EDGE ( 'NONE', *, *, #18959, .F. ) ;
#3043 = FACE_OUTER_BOUND ( 'NONE', #6602, .T. ) ;
#3044 = APPROVAL_STATUS ( 'not_yet_approved' ) ;
#3045 = APPROVAL ( #2020, 'UNSPECIFIED' ) ;
#3046 = DIRECTION ( 'NONE',  ( 0.000000000000000000, 0.000000000000000000, -1.000000000000000000 ) ) ;
#3047 = CARTESIAN_POINT ( 'NONE',  ( 14.48738767196504362, -3581.708301318878966, 2247.301656039307090 ) ) ;
#3048 = AXIS2_PLACEMENT_3D ( 'NONE', #21363, #17950, #10923 ) ;
#3049 = DIRECTION ( 'NONE',  ( -1.224646799147353207E-16, 1.000000000000000000, 0.000000000000000000 ) ) ;
#3050 = AXIS2_PLACEMENT_3D ( 'NONE', #10447, #5188, #19358 ) ;
#3051 = EDGE_CURVE ( 'NONE', #5217, #7352, #10307, .T. ) ;
#3052 = EDGE_CURVE ( 'NONE', #3812, #9191, #6694, .T. ) ;
#3053 = ORIENTED_EDGE ( 'NONE', *, *, #1334, .T. ) ;
#3054 = CARTESIAN_POINT ( 'NONE',  ( 15.70174596903387076, -3695.700000000000273, 2254.617539517497789 ) ) ;
#3055 = EDGE_CURVE ( 'NONE', #19192, #9415, #12206, .T. ) ;
#3056 = LINE ( 'NONE', #11965, #2434 ) ;
#3057 = VERTEX_POINT ( 'NONE', #12305 ) ;
#3058 = CARTESIAN_POINT ( 'NONE',  ( -0.7620000000000000107, -3544.061999999999898, 2254.250000000000000 ) ) ;
#3059 = CARTESIAN_POINT ( 'NONE',  ( 139.6999999999999886, -3576.320000000000164, 2270.760000000000218 ) ) ;
#3060 = ORIENTED_EDGE ( 'NONE', *, *, #2941, .F. ) ;
#3061 = EDGE_CURVE ( 'NONE', #15010, #1694, #17490, .T. ) ;
#3062 = DIRECTION ( 'NONE',  ( 0.000000000000000000, -1.000000000000000000, 0.000000000000000000 ) ) ;
#3063 = B_SPLINE_CURVE_WITH_KNOTS ( 'NONE', 3,
 ( #13408, #18453, #858, #20440, #6275, #4389, #4497, #18338, #978, #14836, #2622, #9767, #15170, #5935, #11631, #18789 ),
 .UNSPECIFIED., .F., .F.,
 ( 4, 2, 2, 2, 2, 2, 2, 4 ),
 ( 0.000000000000000000, 0.0005578396384567584597, 0.001115679276913516919, 0.001673518915370275162, 0.002231358553827033839, 0.003347037830739731101, 0.003904877469195421405, 0.004462717107651111709 ),
 .UNSPECIFIED. ) ;
#3064 = CIRCLE ( 'NONE', #86, 5.460999999999938126 ) ;
#3065 = EDGE_LOOP ( 'NONE', ( #19908, #11118 ) ) ;
#3066 = VECTOR ( 'NONE', #16390, 1000.000000000000000 ) ;
#3067 = CARTESIAN_POINT ( 'NONE',  ( 12.69999999999999929, -3636.327499999999873, 2264.841800000000148 ) ) ;
#3068 = DIRECTION ( 'NONE',  ( 0.000000000000000000, 1.000000000000000000, -1.224646799147353207E-16 ) ) ;
#3069 = CARTESIAN_POINT ( 'NONE',  ( 13.63269303062000048, -3602.191336588000013, 2279.779804022999997 ) ) ;
#3070 = EDGE_CURVE ( 'NONE', #7277, #17151, #22668, .T. ) ;
#3071 = DIRECTION ( 'NONE',  ( 0.7071067811865975328, -3.219513736388853369E-15, -0.7071067811864976127 ) ) ;
#3072 = CALENDAR_DATE ( 2026, 26, 10 ) ;
#3073 = EDGE_CURVE ( 'NONE', #21998, #5163, #20977, .T. ) ;
#3074 = DIRECTION ( 'NONE',  ( -0.8660254037839142383, -0.5000000000009082735, 0.000000000000000000 ) ) ;
#3075 = DIRECTION ( 'NONE',  ( 1.105405881099000035E-12, 1.000000000000000000, 0.000000000000000000 ) ) ;
#3076 = DIRECTION ( 'NONE',  ( -1.000000000000000000, 0.000000000000000000, 0.000000000000000000 ) ) ;
#3077 = AXIS2_PLACEMENT_3D ( 'NONE', #2537, #15190, #20350 ) ;
#3078 = CARTESIAN_POINT ( 'NONE',  ( 141.8201150885594757, -3657.608162431468827, 2248.689186079961019 ) ) ;
#3079 = AXIS2_PLACEMENT_3D ( 'NONE', #5138, #3014, #15677 ) ;
#3080 = ORIENTED_EDGE ( 'NONE', *, *, #3865, .F. ) ;
#3081 = CIRCLE ( 'NONE', #464, 0.7619999999999294005 ) ;
#3082 = CARTESIAN_POINT ( 'NONE',  ( 136.6986430980723242, -3543.300000000018827, 2254.618513951348632 ) ) ;
#3083 = EDGE_CURVE ( 'NONE', #15707, #16281, #17060, .T. ) ;
#3084 = CIRCLE ( 'NONE', #16193, 2.844799999999994444 ) ;
#3085 = ORIENTED_EDGE ( 'NONE', *, *, #762, .F. ) ;
#3086 = CARTESIAN_POINT ( 'NONE',  ( 3.044261469286652755, -3695.700000000080308, 2275.317430734601658 ) ) ;
#3087 = CARTESIAN_POINT ( 'NONE',  ( 127.0000000000000000, -3660.140000000000327, 2244.547199999999975 ) ) ;
#3088 = VERTEX_POINT ( 'NONE', #22949 ) ;
#3089 = ORIENTED_EDGE ( 'NONE', *, *, #20301, .F. ) ;
#3090 = CARTESIAN_POINT ( 'NONE',  ( 98.75520000000000209, -3619.500000000000000, 2261.869999999999891 ) ) ;
#3091 = AXIS2_PLACEMENT_3D ( 'NONE', #19112, #20750, #15603 ) ;
#3092 = CARTESIAN_POINT ( 'NONE',  ( 136.9568000000001291, -3660.383257047432380, 2255.967039999999997 ) ) ;
#3093 = ORIENTED_EDGE ( 'NONE', *, *, #5936, .F. ) ;
#3094 = DIRECTION ( 'NONE',  ( 0.000000000000000000, 0.000000000000000000, 1.000000000000000000 ) ) ;
#3095 = DIRECTION ( 'NONE',  ( 1.000000000000000000, 0.000000000000000000, 0.000000000000000000 ) ) ;
#3096 = CARTESIAN_POINT ( 'NONE',  ( 67.10679999999999268, -3594.099999999999909, 2260.600000000000364 ) ) ;
#3097 = CARTESIAN_POINT ( 'NONE',  ( 14.05634339854999837, -3597.148244321000220, 2296.210799999999836 ) ) ;
#3098 = TOROIDAL_SURFACE ( 'NONE', #11686, 3.606799999999999784, 0.7620000000000000107 ) ;
#3099 = CARTESIAN_POINT ( 'NONE',  ( -6.731000000000118888, -3660.140000000000327, 2242.311999999999898 ) ) ;
#3100 = EDGE_LOOP ( 'NONE', ( #3885, #513, #22647, #2707 ) ) ;
#3101 = APPROVAL_STATUS ( 'not_yet_approved' ) ;
#3102 = AXIS2_PLACEMENT_3D ( 'NONE', #15731, #10573, #12445 ) ;
#3103 = ORIENTED_EDGE ( 'NONE', *, *, #7244, .T. ) ;
#3104 = LINE ( 'NONE', #1461, #4176 ) ;
#3105 = ORIENTED_EDGE ( 'NONE', *, *, #12013, .T. ) ;
#3106 = CARTESIAN_POINT ( 'NONE',  ( 10.31606189812206154, -3581.047200597019582, 2249.211077905966249 ) ) ;
#3107 = FACE_OUTER_BOUND ( 'NONE', #14452, .T. ) ;
#3108 = VERTEX_POINT ( 'NONE', #1279 ) ;
#3109 = AXIS2_PLACEMENT_3D ( 'NONE', #10, #9029, #5176 ) ;
#3110 = DIRECTION ( 'NONE',  ( 0.000000000000000000, 0.000000000000000000, -1.000000000000000000 ) ) ;
#3111 = DIRECTION ( 'NONE',  ( -1.000000000000000000, 0.000000000000000000, 0.000000000000000000 ) ) ;
#3112 = CARTESIAN_POINT ( 'NONE',  ( 145.0370523213743184, -3661.552992845433891, 2244.917889001342246 ) ) ;
#3113 = VECTOR ( 'NONE', #16563, 1000.000000000000000 ) ;
#3114 = CARTESIAN_POINT ( 'NONE',  ( 132.0583097651000060, -3694.797466901999996, 2260.545675974999995 ) ) ;
#3115 = CARTESIAN_POINT ( 'NONE',  ( 10.62862398006557640, -3661.455063412160598, 2249.914674052713508 ) ) ;
#3116 = CLOSED_SHELL ( 'NONE', ( #17229, #11564, #20533, #5705, #12324, #6964, #9811, #8551, #16932, #2489, #13835, #7641, #4021, #6800, #9019, #16453, #5515, #1929, #15278, #8418, #13537, #5023, #16532, #11114, #14265, #19609, #1550, #972, #22940, #1644, #19187, #13238, #14899, #8861, #9921, #14180, #5377, #4836, #5387, #11084, #22107, #498, #6391, #9132, #15882, #12707, #21413, #3800, #8097, #2148 ) ) ;
#3117 = EDGE_CURVE ( 'NONE', #9478, #6254, #8101, .T. ) ;
#3118 = PLANE ( 'NONE',  #19315 ) ;
#3119 = ORIENTED_EDGE ( 'NONE', *, *, #20383, .F. ) ;
#3120 = ADVANCED_FACE ( 'NONE', ( #6916, #13946, #21095 ), #12184, .F. ) ;
#3121 = CARTESIAN_POINT ( 'NONE',  ( 3.048000000000000043, -3544.061999999999898, 2238.248000000000047 ) ) ;
#3122 = CARTESIAN_POINT ( 'NONE',  ( 142.2400000000000091, -3695.699999999999818, 2255.774000000000342 ) ) ;
#3123 = DIRECTION ( 'NONE',  ( 0.000000000000000000, 0.000000000000000000, -1.000000000000000000 ) ) ;
#3124 = CARTESIAN_POINT ( 'NONE',  ( 14.51722411178351813, -3657.316120473550654, 2247.740791187773084 ) ) ;
#3125 = DIRECTION ( 'NONE',  ( -5.682243826821398966E-14, -1.000000000000000000, 0.000000000000000000 ) ) ;
#3126 = ORIENTED_EDGE ( 'NONE', *, *, #15553, .T. ) ;
#3127 = EDGE_CURVE ( 'NONE', #20621, #10571, #6305, .T. ) ;
#3128 = AXIS2_PLACEMENT_3D ( 'NONE', #17547, #9324, #5025 ) ;
#3129 = VERTEX_POINT ( 'NONE', #20356 ) ;
#3130 = DIRECTION ( 'NONE',  ( 0.000000000000000000, 0.000000000000000000, -1.000000000000000000 ) ) ;
#3131 = ORIENTED_EDGE ( 'NONE', *, *, #20397, .F. ) ;
#3132 = CYLINDRICAL_SURFACE ( 'NONE', #16749, 1.270000000000000018 ) ;
#3133 = COORDINATED_UNIVERSAL_TIME_OFFSET ( 0, 0, .AHEAD. ) ;
#3134 = EDGE_CURVE ( 'NONE', #3129, #17497, #23054, .T. ) ;
#3135 = DIRECTION ( 'NONE',  ( 0.000000000000000000, 0.000000000000000000, -1.000000000000000000 ) ) ;
#3136 = VERTEX_POINT ( 'NONE', #22212 ) ;
#3137 = EDGE_CURVE ( 'NONE', #20690, #21069, #12340, .T. ) ;
#3138 = CARTESIAN_POINT ( 'NONE',  ( 142.1683190434573305, -3578.068567422205888, 2257.869726352968428 ) ) ;
#3139 = DIRECTION ( 'NONE',  ( -5.682243826821398966E-14, -1.000000000000000000, 0.000000000000000000 ) ) ;
#3140 = CARTESIAN_POINT ( 'NONE',  ( 14.03517516284999900, -3656.987758144000054, 2257.672197071000028 ) ) ;
#3141 = CARTESIAN_POINT ( 'NONE',  ( 12.69999999999999929, -3574.034000000000106, 2239.391000000000076 ) ) ;
#3142 = CARTESIAN_POINT ( 'NONE',  ( 116.8400000000000034, -3543.299999999999727, 2247.392000000000280 ) ) ;
#3143 = VERTEX_POINT ( 'NONE', #22103 ) ;
#3144 = CIRCLE ( 'NONE', #7269, 2.844800000000091700 ) ;
#3145 = DIRECTION ( 'NONE',  ( -1.000000000000000000, 0.000000000000000000, 0.000000000000000000 ) ) ;
#3146 = CARTESIAN_POINT ( 'NONE',  ( -12.31900000000000084, -3576.510744320999947, 2246.035656601000028 ) ) ;
#3147 = AXIS2_PLACEMENT_3D ( 'NONE', #16949, #2440, #14976 ) ;
#3148 = EDGE_LOOP ( 'NONE', ( #16205, #11478, #10065, #4548 ) ) ;
#3149 = DIRECTION ( 'NONE',  ( -1.159746789738050283E-14, -0.5000000000005221379, 0.8660254037841371710 ) ) ;
#3150 = CARTESIAN_POINT ( 'NONE',  ( 10.05102782082138901, -3658.467715238130495, 2249.693416503429489 ) ) ;
#3151 = ORIENTED_EDGE ( 'NONE', *, *, #22542, .T. ) ;
#3152 = PLANE ( 'NONE',  #20294 ) ;
#3153 = ORIENTED_EDGE ( 'NONE', *, *, #21141, .T. ) ;
#3154 = PERSON_AND_ORGANIZATION_ROLE ( 'creator' ) ;
#3155 = CYLINDRICAL_SURFACE ( 'NONE', #13555, 0.3810000000000011156 ) ;
#3156 = EDGE_LOOP ( 'NONE', ( #12594, #412 ) ) ;
#3157 = DIRECTION ( 'NONE',  ( 0.5000000000007065459, 0.8660254037840305896, 0.000000000000000000 ) ) ;
#3158 = AXIS2_PLACEMENT_3D ( 'NONE', #2432, #9575, #16721 ) ;
#3159 = SECURITY_CLASSIFICATION_LEVEL ( 'unclassified' ) ;
#3160 = AXIS2_PLACEMENT_3D ( 'NONE', #2467, #9387, #7744 ) ;
#3161 = CIRCLE ( 'NONE', #16272, 1.269999999999882334 ) ;
#3162 = DIRECTION ( 'NONE',  ( 1.000000000000000000, 0.000000000000000000, 0.000000000000000000 ) ) ;
#3163 = CARTESIAN_POINT ( 'NONE',  ( 14.67418966406092906, -3581.543406057290667, 2248.337984869423053 ) ) ;
#3164 = CARTESIAN_POINT ( 'NONE',  ( 134.0156995028073652, -3658.912717518575846, 2244.825196086624601 ) ) ;
#3165 = DIRECTION ( 'NONE',  ( -1.000000000000000000, 0.000000000000000000, 0.000000000000000000 ) ) ;
#3166 = ORIENTED_EDGE ( 'NONE', *, *, #9981, .T. ) ;
#3167 = DIRECTION ( 'NONE',  ( 0.000000000000000000, 1.000000000000000000, 0.000000000000000000 ) ) ;
#3168 = CARTESIAN_POINT ( 'NONE',  ( 13.24918551347000140, -3576.699137200999758, 2257.605105471000115 ) ) ;
#3169 = ORIENTED_EDGE ( 'NONE', *, *, #10690, .T. ) ;
#3170 = AXIS2_PLACEMENT_3D ( 'NONE', #14577, #21719, #21836 ) ;
#3171 = DIRECTION ( 'NONE',  ( 0.000000000000000000, 0.000000000000000000, -1.000000000000000000 ) ) ;
#3172 = VECTOR ( 'NONE', #3517, 1000.000000000000000 ) ;
#3173 = APPLIED_PERSON_AND_ORGANIZATION_ASSIGNMENT ( #1991, #14649, ( #10864 ) ) ;
#3174 = VECTOR ( 'NONE', #6796, 1000.000000000000000 ) ;
#3175 = FACE_OUTER_BOUND ( 'NONE', #5544, .T. ) ;
#3176 = AXIS2_PLACEMENT_3D ( 'NONE', #18766, #22275, #22167 ) ;
#3177 = ORIENTED_EDGE ( 'NONE', *, *, #17604, .F. ) ;
#3178 = DIRECTION ( 'NONE',  ( 0.000000000000000000, 0.000000000000000000, -1.000000000000000000 ) ) ;
#3179 = CARTESIAN_POINT ( 'NONE',  ( 134.0023458843163269, -3659.955155772517628, 2244.552343395693697 ) ) ;
#3180 = VERTEX_POINT ( 'NONE', #6414 ) ;
#3181 = DIRECTION ( 'NONE',  ( -1.000000000000000000, 0.000000000000000000, 0.000000000000000000 ) ) ;
#3182 = CARTESIAN_POINT ( 'NONE',  ( 15.48441936004095609, -3660.088012435405744, 2250.236355021178952 ) ) ;
#3183 = EDGE_CURVE ( 'NONE', #21998, #5432, #15957, .T. ) ;
#3184 = DIRECTION ( 'NONE',  ( 0.000000000000000000, 0.000000000000000000, -1.000000000000000000 ) ) ;
#3185 = PERSON ( 'NAUO-PER1', 'UNSPECIFIED', 'UNSPECIFIED', ('UNSPECIFIED'), ('UNSPECIFIED'), ('UNSPECIFIED') ) ;
#3186 = DIRECTION ( 'NONE',  ( 1.000000000000000000, 0.000000000000000000, 0.000000000000000000 ) ) ;
#3187 = PERSON_AND_ORGANIZATION ( #5446, #1895 ) ;
#3188 = EDGE_CURVE ( 'NONE', #1907, #22946, #15631, .T. ) ;
#3189 = CARTESIAN_POINT ( 'NONE',  ( 139.7000000001000046, -3656.372659094999563, 2239.009999999999764 ) ) ;
#3190 = CARTESIAN_POINT ( 'NONE',  ( 12.69999999999999929, -3590.289999999999964, 2268.705139999999574 ) ) ;
#3191 = CARTESIAN_POINT ( 'NONE',  ( 123.3932000000010021, -3619.500000000000000, 2239.009999999999764 ) ) ;
#3192 = VECTOR ( 'NONE', #8691, 1000.000000000000000 ) ;
#3193 = AXIS2_PLACEMENT_3D ( 'NONE', #472, #7614, #14773 ) ;
#3194 = PRODUCT ( 'Screw 4', 'Screw 4', '', ( #1815 ) ) ;
#3195 = CARTESIAN_POINT ( 'NONE',  ( 141.6086330389385353, -3657.395487126937496, 2248.141035207103869 ) ) ;
#3196 = VECTOR ( 'NONE', #7032, 1000.000000000000000 ) ;
#3197 = EDGE_LOOP ( 'NONE', ( #20907, #13516, #18847, #11703, #4967, #1479, #15417, #4245 ) ) ;
#3198 =( BOUNDED_CURVE ( )  B_SPLINE_CURVE ( 3, ( #16474, #9560, #4713, #21979 ),
 .UNSPECIFIED., .F., .T. ) 
 B_SPLINE_CURVE_WITH_KNOTS ( ( 4, 4 ),
 ( -2.664535259100375697E-14, 1.570796326276726607 ),
 .UNSPECIFIED. ) 
 CURVE ( )  GEOMETRIC_REPRESENTATION_ITEM ( )  RATIONAL_B_SPLINE_CURVE ( ( 1.000000000000000000, 0.8047378542464924678, 0.8047378542464924678, 1.000000000000000000 ) ) 
 REPRESENTATION_ITEM ( '' )  );
#3199 = DIRECTION ( 'NONE',  ( 1.224646799147353207E-16, 1.000000000000000000, -0.000000000000000000 ) ) ;
#3200 = ORIENTED_EDGE ( 'NONE', *, *, #8644, .T. ) ;
#3201 = ORIENTED_EDGE ( 'NONE', *, *, #11389, .T. ) ;
#3202 = PLANE ( 'NONE',  #20756 ) ;
#3203 = EDGE_LOOP ( 'NONE', ( #7978, #20087, #11756, #156 ) ) ;
#3204 = ORIENTED_EDGE ( 'NONE', *, *, #21878, .T. ) ;
#3205 = DIRECTION ( 'NONE',  ( -0.7071067811865975328, 0.000000000000000000, -0.7071067811864976127 ) ) ;
#3206 = CIRCLE ( 'NONE', #5096, 11.11250000000000071 ) ;
#3207 = COORDINATED_UNIVERSAL_TIME_OFFSET ( 0, 0, .AHEAD. ) ;
#3208 = LINE ( 'NONE', #13881, #2056 ) ;
#3209 = AXIS2_PLACEMENT_3D ( 'NONE', #13325, #9580, #6308 ) ;
#3210 = DIRECTION ( 'NONE',  ( -2.330758767202000237E-14, -1.000000000000000000, -1.224646799141892318E-16 ) ) ;
#3211 = VERTEX_POINT ( 'NONE', #16943 ) ;
#3212 = CIRCLE ( 'NONE', #23047, 2.844800000000001550 ) ;
#3213 = FACE_OUTER_BOUND ( 'NONE', #14947, .T. ) ;
#3214 = EDGE_CURVE ( 'NONE', #7868, #8256, #6533, .T. ) ;
#3215 = DIRECTION ( 'NONE',  ( 0.000000000000000000, 0.000000000000000000, 1.000000000000000000 ) ) ;
#3216 = CARTESIAN_POINT ( 'NONE',  ( 18.16100000000000136, -3639.502500000000055, 2296.210799999999836 ) ) ;
#3217 = CARTESIAN_POINT ( 'NONE',  ( -8.890000000032001637, -3658.793800000000374, 2245.060313203000078 ) ) ;
#3218 = AXIS2_PLACEMENT_3D ( 'NONE', #8395, #13428, #15424 ) ;
#3219 = EDGE_CURVE ( 'NONE', #11141, #5364, #14845, .T. ) ;
#3220 = VERTEX_POINT ( 'NONE', #6184 ) ;
#3221 = PERSON_AND_ORGANIZATION ( #5446, #1895 ) ;
#3222 = EDGE_CURVE ( 'NONE', #7743, #4703, #17828, .T. ) ;
#3223 = ORIENTED_EDGE ( 'NONE', *, *, #2554, .F. ) ;
#3224 = VECTOR ( 'NONE', #15591, 1000.000000000000000 ) ;
#3225 = VECTOR ( 'NONE', #1470, 1000.000000000000000 ) ;
#3226 = DIRECTION ( 'NONE',  ( 0.000000000000000000, -1.000000000000000000, 0.000000000000000000 ) ) ;
#3227 = CARTESIAN_POINT ( 'NONE',  ( 10.90747266517406011, -3581.704041953448268, 2247.289616970143470 ) ) ;
#3228 = DIRECTION ( 'NONE',  ( -1.000000000000000000, 0.000000000000000000, 0.000000000000000000 ) ) ;
#3229 = ORIENTED_EDGE ( 'NONE', *, *, #4364, .F. ) ;
#3230 = VERTEX_POINT ( 'NONE', #20574 ) ;
#3231 = FACE_OUTER_BOUND ( 'NONE', #15368, .T. ) ;
#3232 = AXIS2_PLACEMENT_3D ( 'NONE', #8008, #16897, #22056 ) ;
#3233 = CARTESIAN_POINT ( 'NONE',  ( 20.32000000000000028, -3694.938000000000102, 2289.213099999999940 ) ) ;
#3234 = CARTESIAN_POINT ( 'NONE',  ( 15.03168679717000167, -3580.841199999999844, 2242.820000000000164 ) ) ;
#3235 = CARTESIAN_POINT ( 'NONE',  ( 50.79999999999999716, -3568.700000000000273, 2259.837999999999738 ) ) ;
#3236 = AXIS2_PLACEMENT_3D ( 'NONE', #12461, #3199, #19608 ) ;
#3237 = DIRECTION ( 'NONE',  ( 0.000000000000000000, -1.000000000000000000, 0.000000000000000000 ) ) ;
#3238 = LINE ( 'NONE', #8401, #4699 ) ;
#3239 = AXIS2_PLACEMENT_3D ( 'NONE', #12375, #1471, #13906 ) ;
#3240 = ORIENTED_EDGE ( 'NONE', *, *, #13995, .T. ) ;
#3241 = DIRECTION ( 'NONE',  ( -1.000000000000000000, 0.000000000000000000, 0.000000000000000000 ) ) ;
#3242 = CARTESIAN_POINT ( 'NONE',  ( 12.69999999997255280, -3636.370159094721657, 2296.591799999999694 ) ) ;
#3243 = CARTESIAN_POINT ( 'NONE',  ( 134.0203227398999957, -3578.860230781999689, 2244.548186305999934 ) ) ;
#3244 = LINE ( 'NONE', #1477, #1976 ) ;
#3245 = CARTESIAN_POINT ( 'NONE',  ( 50.79999999999999716, -3619.500000000000000, 2259.837999999999738 ) ) ;
#3246 = ORIENTED_EDGE ( 'NONE', *, *, #18195, .T. ) ;
#3247 = ORIENTED_EDGE ( 'NONE', *, *, #11813, .T. ) ;
#3248 = EDGE_CURVE ( 'NONE', #7121, #16307, #9906, .T. ) ;
#3249 = CIRCLE ( 'NONE', #11121, 3.606799999998994366 ) ;
#3250 = ORIENTED_EDGE ( 'NONE', *, *, #19700, .T. ) ;
#3251 = AXIS2_PLACEMENT_3D ( 'NONE', #12888, #5756, #21794 ) ;
#3252 = CARTESIAN_POINT ( 'NONE',  ( 14.71507054554999883, -3581.509743952999997, 2257.776232814999730 ) ) ;
#3253 = PERSON_AND_ORGANIZATION_ROLE ( 'classification_officer' ) ;
#3254 = EDGE_CURVE ( 'NONE', #6140, #14734, #21757, .T. ) ;
#3255 = PLANE ( 'NONE',  #7573 ) ;
#3256 = EDGE_CURVE ( 'NONE', #11901, #10278, #11660, .T. ) ;
#3257 = CARTESIAN_POINT ( 'NONE',  ( 12.15081356636999921, -3656.709137308999743, 2257.605105499000274 ) ) ;
#3258 = CARTESIAN_POINT ( 'NONE',  ( 9.855200958505918152, -3659.596994900638038, 2257.962940081783472 ) ) ;
#3259 = DIRECTION ( 'NONE',  ( 0.000000000000000000, 0.000000000000000000, -1.000000000000000000 ) ) ;
#3260 = CARTESIAN_POINT ( 'NONE',  ( 142.5447999999989861, -3659.504999999999654, 2272.030000000000200 ) ) ;
#3261 = EDGE_CURVE ( 'NONE', #20781, #20823, #17078, .T. ) ;
#3262 = ORIENTED_EDGE ( 'NONE', *, *, #20859, .F. ) ;
#3263 = PLANE ( 'NONE',  #17405 ) ;
#3264 = DIRECTION ( 'NONE',  ( 0.000000000000000000, -1.000000000000000000, 0.000000000000000000 ) ) ;
#3265 = ORIENTED_EDGE ( 'NONE', *, *, #15360, .T. ) ;
#3266 = CARTESIAN_POINT ( 'NONE',  ( 95.25000000000000000, -3695.699999999999818, 2243.277199999999993 ) ) ;
#3267 = CARTESIAN_POINT ( 'NONE',  ( 10.59562833397165171, -3657.590649014947303, 2248.654563546086138 ) ) ;
#3268 = ADVANCED_FACE ( 'NONE', ( #4763 ), #2999, .T. ) ;
#3269 = EDGE_CURVE ( 'NONE', #21296, #13145, #13200, .T. ) ;
#3270 = VECTOR ( 'NONE', #7761, 1000.000000000000000 ) ;
#3271 = VERTEX_POINT ( 'NONE', #11444 ) ;
#3272 = DIRECTION ( 'NONE',  ( 1.224646799147353207E-16, 1.000000000000000000, -0.000000000000000000 ) ) ;
#3273 = ORIENTED_EDGE ( 'NONE', *, *, #16870, .T. ) ;
#3274 = EDGE_LOOP ( 'NONE', ( #2308, #13362 ) ) ;
#3275 = CARTESIAN_POINT ( 'NONE',  ( 15.87500000000000000, -3543.299999999999727, 2281.351799999999912 ) ) ;
#3276 = PERSON_AND_ORGANIZATION ( #5446, #1895 ) ;
#3277 = AXIS2_PLACEMENT_3D ( 'NONE', #18323, #2045, #9314 ) ;
#3278 = DIRECTION ( 'NONE',  ( 0.000000000000000000, -1.000000000000000000, 0.000000000000000000 ) ) ;
#3279 = ORIENTED_EDGE ( 'NONE', *, *, #13685, .T. ) ;
#3280 = CARTESIAN_POINT ( 'NONE',  ( 14.05634339854999837, -3637.153244320999875, 2296.210799999999836 ) ) ;
#3281 = APPROVAL_DATE_TIME ( #19342, #11201 ) ;
#3282 = VECTOR ( 'NONE', #12975, 1000.000000000000000 ) ;
#3283 = EDGE_CURVE ( 'NONE', #9572, #19328, #7733, .T. ) ;
#3284 = CARTESIAN_POINT ( 'NONE',  ( 97.99320000000000164, -3568.700000000000273, 2239.771999999999935 ) ) ;
#3285 = DIRECTION ( 'NONE',  ( 0.000000000000000000, -1.000000000000000000, 0.000000000000000000 ) ) ;
#3286 = DIRECTION ( 'NONE',  ( 0.000000000000000000, 0.000000000000000000, -1.000000000000000000 ) ) ;
#3287 = AXIS2_PLACEMENT_3D ( 'NONE', #1083, #6148, #4488 ) ;
#3288 = DIRECTION ( 'NONE',  ( 0.000000000000000000, 0.000000000000000000, -1.000000000000000000 ) ) ;
#3289 = CARTESIAN_POINT ( 'NONE',  ( 127.0000000000000000, -3578.860000000000127, 2247.392000000000280 ) ) ;
#3290 = ORIENTED_EDGE ( 'NONE', *, *, #11778, .T. ) ;
#3291 = CARTESIAN_POINT ( 'NONE',  ( 15.55727146409452821, -3695.607672421357620, 2254.979487869122295 ) ) ;
#3292 = CARTESIAN_POINT ( 'NONE',  ( -12.54218463257233118, -3576.167599999590948, 2247.391999999993914 ) ) ;
#3293 = ORIENTED_EDGE ( 'NONE', *, *, #15391, .F. ) ;
#3294 = DIRECTION ( 'NONE',  ( 0.000000000000000000, 0.000000000000000000, -1.000000000000000000 ) ) ;
#3295 = EDGE_CURVE ( 'NONE', #5223, #11524, #23067, .T. ) ;
#3296 = DIRECTION ( 'NONE',  ( 0.000000000000000000, 0.000000000000000000, -1.000000000000000000 ) ) ;
#3297 = ORIENTED_EDGE ( 'NONE', *, *, #18597, .T. ) ;
#3298 = VERTEX_POINT ( 'NONE', #9794 ) ;
#3299 = CARTESIAN_POINT ( 'NONE',  ( 15.54479999999999862, -3599.497499999999945, 2281.351799999999912 ) ) ;
#3300 = DIRECTION ( 'NONE',  ( 0.000000000000000000, 0.000000000000000000, -1.000000000000000000 ) ) ;
#3301 = VERTEX_POINT ( 'NONE', #882 ) ;
#3302 = CARTESIAN_POINT ( 'NONE',  ( -12.31900000000000084, -3580.206200000121044, 2249.723686796789480 ) ) ;
#3303 = PLANE ( 'NONE',  #14254 ) ;
#3304 =( LENGTH_UNIT ( ) NAMED_UNIT ( * ) SI_UNIT ( .MILLI., .METRE. ) );
#3305 = DIRECTION ( 'NONE',  ( 0.7249994335945011414, 6.337882393833011158E-14, 0.6887494619146010688 ) ) ;
#3306 = COORDINATED_UNIVERSAL_TIME_OFFSET ( 0, 0, .AHEAD. ) ;
#3307 = DIRECTION ( 'NONE',  ( 2.294752314678193758E-12, 0.000000000000000000, 1.000000000000000000 ) ) ;
#3308 = FACE_OUTER_BOUND ( 'NONE', #15006, .T. ) ;
#3309 = CARTESIAN_POINT ( 'NONE',  ( 18.36105254568060019, -3580.284312841101382, 2244.927052815691695 ) ) ;
#3310 = CARTESIAN_POINT ( 'NONE',  ( 141.6126669512999854, -3657.399152860999493, 2246.630000000000109 ) ) ;
#3311 = EDGE_LOOP ( 'NONE', ( #5703, #20308, #885, #21896 ) ) ;
#3312 = AXIS2_PLACEMENT_3D ( 'NONE', #5858, #18707, #18486 ) ;
#3313 = DIRECTION ( 'NONE',  ( 1.000000000000000000, 0.000000000000000000, 0.000000000000000000 ) ) ;
#3314 = ORIENTED_EDGE ( 'NONE', *, *, #9099, .F. ) ;
#3315 = ORIENTED_EDGE ( 'NONE', *, *, #22331, .T. ) ;
#3316 = VERTEX_POINT ( 'NONE', #3346 ) ;
#3317 = DIRECTION ( 'NONE',  ( -2.324635735433000053E-14, 2.336881798971000105E-14, -1.000000000000000000 ) ) ;
#3318 = EDGE_LOOP ( 'NONE', ( #3707, #135, #3279, #3349 ) ) ;
#3319 = ORIENTED_EDGE ( 'NONE', *, *, #2265, .F. ) ;
#3320 = CARTESIAN_POINT ( 'NONE',  ( 4.878250543320599597, -3543.555041885565970, 2260.094480151607968 ) ) ;
#3321 = ITEM_DEFINED_TRANSFORMATION ( 'NONE', 'NONE', #14,  #5611 ) ;
#3322 = DIRECTION ( 'NONE',  ( 0.000000000000000000, 0.000000000000000000, -1.000000000000000000 ) ) ;
#3323 = CARTESIAN_POINT ( 'NONE',  ( -12.31899999999988005, -3578.860000000000127, 2252.472000000000207 ) ) ;
#3324 = ORIENTED_EDGE ( 'NONE', *, *, #6354, .T. ) ;
#3325 = CARTESIAN_POINT ( 'NONE',  ( 7.619999999999999218, -3659.504999999999654, 2244.978999999999814 ) ) ;
#3326 = CARTESIAN_POINT ( 'NONE',  ( 63.50000000000000000, -3594.099999999999909, 2259.837999999999738 ) ) ;
#3327 = CARTESIAN_POINT ( 'NONE',  ( 25.39999999999999858, -3619.500000000000000, 2260.600000000000364 ) ) ;
#3328 = CIRCLE ( 'NONE', #15686, 5.460999999999938126 ) ;
#3329 = CARTESIAN_POINT ( 'NONE',  ( 0.000000000000000000, -3578.860000000000127, 2243.785200000000259 ) ) ;
#3330 = ORIENTED_EDGE ( 'NONE', *, *, #14544, .F. ) ;
#3331 = PERSON_AND_ORGANIZATION ( #5446, #1895 ) ;
#3332 = VERTEX_POINT ( 'NONE', #13791 ) ;
#3333 = CARTESIAN_POINT ( 'NONE',  ( 18.41500000000100101, -3579.494999999999891, 2239.771999999999935 ) ) ;
#3334 =( BOUNDED_CURVE ( )  B_SPLINE_CURVE ( 3, ( #19949, #21701, #11035, #7520 ),
 .UNSPECIFIED., .F., .T. ) 
 B_SPLINE_CURVE_WITH_KNOTS ( ( 4, 4 ),
 ( 3.673835071120113713E-14, 1.570796326419416467 ),
 .UNSPECIFIED. ) 
 CURVE ( )  GEOMETRIC_REPRESENTATION_ITEM ( )  RATIONAL_B_SPLINE_CURVE ( ( 1.000000000000000000, 0.8047378542128751366, 0.8047378542128751366, 1.000000000000000000 ) ) 
 REPRESENTATION_ITEM ( '' )  );
#3335 = APPLIED_PERSON_AND_ORGANIZATION_ASSIGNMENT ( #660, #872, ( #13121 ) ) ;
#3336 = CARTESIAN_POINT ( 'NONE',  ( 10.87628247337022636, -3581.678378035377136, 2246.973460001757303 ) ) ;
#3337 = ORIENTED_EDGE ( 'NONE', *, *, #1656, .T. ) ;
#3338 = CARTESIAN_POINT ( 'NONE',  ( -5.588000000000000078, -3544.061999999999898, 2253.487999999999829 ) ) ;
#3339 = ORIENTED_EDGE ( 'NONE', *, *, #14329, .F. ) ;
#3340 = DIRECTION ( 'NONE',  ( 0.000000000000000000, 0.000000000000000000, 1.000000000000000000 ) ) ;
#3341 = AXIS2_PLACEMENT_3D ( 'NONE', #17167, #22555, #6526 ) ;
#3342 = EDGE_CURVE ( 'NONE', #16219, #14242, #13720, .T. ) ;
#3343 = EDGE_CURVE ( 'NONE', #6627, #22920, #12983, .T. ) ;
#3344 = DIRECTION ( 'NONE',  ( 0.000000000000000000, 0.000000000000000000, 1.000000000000000000 ) ) ;
#3345 = CARTESIAN_POINT ( 'NONE',  ( 12.69999999999999929, -3579.494999999999891, 2272.030000000000200 ) ) ;
#3346 = CARTESIAN_POINT ( 'NONE',  ( 12.69999999999999929, -3655.060000000000400, 2275.055139999999483 ) ) ;
#3347 = CARTESIAN_POINT ( 'NONE',  ( 12.63689026076125721, -3662.349833683567795, 2249.183488215769103 ) ) ;
#3349 = ORIENTED_EDGE ( 'NONE', *, *, #15885, .F. ) ;
#3348 = ADVANCED_FACE ( 'NONE', ( #23026 ), #12491, .T. ) ;
#3350 = APPLICATION_CONTEXT ( 'configuration controlled 3d designs of mechanical parts and assemblies' ) ;
#3351 = CARTESIAN_POINT ( 'NONE',  ( 136.9873132028999976, -3581.061170452999704, 2239.009999999999764 ) ) ;
#3352 = EDGE_LOOP ( 'NONE', ( #20811, #2532 ) ) ;
#3353 = DIRECTION ( 'NONE',  ( 0.000000000000000000, 0.000000000000000000, -1.000000000000000000 ) ) ;
#3354 = DIRECTION ( 'NONE',  ( 0.000000000000000000, 0.000000000000000000, -1.000000000000000000 ) ) ;
#3355 = DIRECTION ( 'NONE',  ( 0.5000000000031962211, 0.8660254037825932949, 0.000000000000000000 ) ) ;
#3356 = CARTESIAN_POINT ( 'NONE',  ( 14.84429988771011466, -3657.635452944057306, 2248.741321748801511 ) ) ;
#3357 = EDGE_CURVE ( 'NONE', #17996, #21912, #19296, .T. ) ;
#3358 = LINE ( 'NONE', #18006, #467 ) ;
#3359 = EDGE_CURVE ( 'NONE', #20703, #2146, #17452, .T. ) ;
#3360 = DIRECTION ( 'NONE',  ( 0.000000000000000000, 0.000000000000000000, -1.000000000000000000 ) ) ;
#3361 = ORIENTED_EDGE ( 'NONE', *, *, #17352, .F. ) ;
#3362 = DIRECTION ( 'NONE',  ( 0.000000000000000000, 0.000000000000000000, 1.000000000000000000 ) ) ;
#3363 = SECURITY_CLASSIFICATION ( '', '', #20180 ) ;
#3364 = ADVANCED_FACE ( 'NONE', ( #16009 ), #15594, .T. ) ;
#3365 = DIRECTION ( 'NONE',  ( -1.000000000000000000, 5.461016542361937364E-28, 2.336881798970999789E-14 ) ) ;
#3366 = CONTEXT_DEPENDENT_SHAPE_REPRESENTATION ( #20552, #6241 ) ;
#3367 = DIRECTION ( 'NONE',  ( 1.000000000000000000, 0.000000000000000000, 0.000000000000000000 ) ) ;
#3368 = CARTESIAN_POINT ( 'NONE',  ( 20.32000000000000028, -3694.938000000000102, 2292.819899999999961 ) ) ;
#3369 = FACE_BOUND ( 'NONE', #4155, .T. ) ;
#3370 = DIRECTION ( 'NONE',  ( -1.000000000000000000, 0.000000000000000000, 0.000000000000000000 ) ) ;
#3371 = CARTESIAN_POINT ( 'NONE',  ( 139.6999999999999886, -3579.494999999999891, 2272.030000000000200 ) ) ;
#3372 = DIRECTION ( 'NONE',  ( 0.000000000000000000, 0.000000000000000000, -1.000000000000000000 ) ) ;
#3373 = ORIENTED_EDGE ( 'NONE', *, *, #1236, .T. ) ;
#3374 = DIRECTION ( 'NONE',  ( 0.000000000000000000, 0.000000000000000000, -1.000000000000000000 ) ) ;
#3375 = EDGE_CURVE ( 'NONE', #8201, #2255, #10345, .T. ) ;
#3376 = DIRECTION ( 'NONE',  ( -1.000000000000000000, 2.330758767201999921E-14, 2.343004830739999973E-14 ) ) ;
#3377 = ORIENTED_EDGE ( 'NONE', *, *, #15866, .F. ) ;
#3378 = APPLIED_APPROVAL_ASSIGNMENT ( #7348, ( #10864 ) ) ;
#3379 = LINE ( 'NONE', #17554, #14801 ) ;
#3380 = APPLIED_SECURITY_CLASSIFICATION_ASSIGNMENT ( #3761, ( #13121 ) ) ;
#3381 = EDGE_CURVE ( 'NONE', #2645, #17031, #13342, .T. ) ;
#3382 = ADVANCED_FACE ( 'NONE', ( #17760 ), #18577, .T. ) ;
#3383 = CIRCLE ( 'NONE', #19483, 0.7620000000000001217 ) ;
#3384 = ORIENTED_EDGE ( 'NONE', *, *, #13984, .F. ) ;
#3385 = CIRCLE ( 'NONE', #12745, 5.080000000000000959 ) ;
#3386 = CARTESIAN_POINT ( 'NONE',  ( 132.1456718464000062, -3694.678775005999796, 2260.506484774000000 ) ) ;
#3387 = ORIENTED_EDGE ( 'NONE', *, *, #9144, .F. ) ;
#3388 = PRODUCT_DEFINITION_SHAPE ( 'NONE', 'NONE',  #3469 ) ;
#3389 = DIRECTION ( 'NONE',  ( 0.6723379328151413148, 0.7402443543167774864, 0.000000000000000000 ) ) ;
#3390 = CALENDAR_DATE ( 2026, 26, 10 ) ;
#3391 = LINE ( 'NONE', #15596, #18095 ) ;
#3392 = ORIENTED_EDGE ( 'NONE', *, *, #22743, .T. ) ;
#3393 = CARTESIAN_POINT ( 'NONE',  ( 137.2316813306051131, -3580.921433171091394, 2257.869726269903367 ) ) ;
#3394 = PERSON_AND_ORGANIZATION_ROLE ( 'classification_officer' ) ;
#3395 = DIRECTION ( 'NONE',  ( -3.156802126040999989E-13, 2.590196616237999979E-13, -1.000000000000000000 ) ) ;
#3396 = SECURITY_CLASSIFICATION ( '', '', #12742 ) ;
#3397 = DIRECTION ( 'NONE',  ( 1.000000000000000000, 0.000000000000000000, 0.000000000000000000 ) ) ;
#3398 = LOCAL_TIME ( 17, 37, 43.00000000000000000, #6989 ) ;
#3399 = EDGE_CURVE ( 'NONE', #21490, #18111, #3663, .T. ) ;
#3400 = CARTESIAN_POINT ( 'NONE',  ( 14.05634339857000015, -3601.846755679000125, 2296.210799999999836 ) ) ;
#3401 = CARTESIAN_POINT ( 'NONE',  ( 11.34365660141000021, -3641.851755678999780, 2296.210799999999836 ) ) ;
#3402 = DIRECTION ( 'NONE',  ( 0.000000000000000000, 0.000000000000000000, 1.000000000000000000 ) ) ;
#3403 = ORIENTED_EDGE ( 'NONE', *, *, #5149, .T. ) ;
#3404 = FACE_OUTER_BOUND ( 'NONE', #8035, .T. ) ;
#3405 = AXIS2_PLACEMENT_3D ( 'NONE', #20547, #13294, #18573 ) ;
#3406 = CARTESIAN_POINT ( 'NONE',  ( 151.1299999999999955, -3578.860000000000127, 2247.392000000000280 ) ) ;
#3407 = EDGE_LOOP ( 'NONE', ( #21322, #4039 ) ) ;
#3408 = CARTESIAN_POINT ( 'NONE',  ( -12.31900000000000084, -3660.140000000000327, 2247.392000000000280 ) ) ;
#3409 = EDGE_CURVE ( 'NONE', #10931, #16647, #22682, .T. ) ;
#3410 = ADVANCED_FACE ( 'NONE', ( #21054 ), #14257, .T. ) ;
#3411 = CARTESIAN_POINT ( 'NONE',  ( 20.17309679552000290, -3544.443975155000317, 2260.454626673999883 ) ) ;
#3412 = ORIENTED_EDGE ( 'NONE', *, *, #14392, .F. ) ;
#3413 = ADVANCED_FACE ( 'NONE', ( #19637 ), #3580, .F. ) ;
#3414 = FACE_OUTER_BOUND ( 'NONE', #8268, .T. ) ;
#3415 = DIRECTION ( 'NONE',  ( 0.000000000000000000, -1.000000000000000000, 0.000000000000000000 ) ) ;
#3416 = VERTEX_POINT ( 'NONE', #6655 ) ;
#3417 = DIRECTION ( 'NONE',  ( 1.224646799147353207E-16, 1.000000000000000000, -0.000000000000000000 ) ) ;
#3418 = CYLINDRICAL_SURFACE ( 'NONE', #1505, 1.270000000000000018 ) ;
#3419 =( NAMED_UNIT ( * ) PLANE_ANGLE_UNIT ( ) SI_UNIT ( $, .RADIAN. ) );
#3420 = EDGE_CURVE ( 'NONE', #13646, #20939, #5902, .T. ) ;
#3422 = DIRECTION ( 'NONE',  ( 0.000000000000000000, 0.000000000000000000, 1.000000000000000000 ) ) ;
#3421 = AXIS2_PLACEMENT_3D ( 'NONE', #19781, #14509, #1844 ) ;
#3423 = APPROVAL_ROLE ( '' ) ;
#3424 = AXIS2_PLACEMENT_3D ( 'NONE', #8581, #10093, #13852 ) ;
#3425 = DIRECTION ( 'NONE',  ( 1.000000000000000000, 0.000000000000000000, 0.000000000000000000 ) ) ;
#3426 = FACE_BOUND ( 'NONE', #22361, .T. ) ;
#3427 = CARTESIAN_POINT ( 'NONE',  ( 20.32000000000000028, -3544.061999999999898, 2286.368300000000090 ) ) ;
#3428 = ADVANCED_FACE ( 'NONE', ( #22906 ), #8500, .T. ) ;
#3429 = DIRECTION ( 'NONE',  ( 0.000000000000000000, 0.000000000000000000, -1.000000000000000000 ) ) ;
#3430 = EDGE_CURVE ( 'NONE', #2806, #6290, #11126, .T. ) ;
#3431 = ORIENTED_EDGE ( 'NONE', *, *, #7578, .F. ) ;
#3432 = CARTESIAN_POINT ( 'NONE',  ( 15.03168679707239441, -3640.848700000039116, 2296.210799999999836 ) ) ;
#3433 = ORIENTED_EDGE ( 'NONE', *, *, #21311, .T. ) ;
#3434 = ORIENTED_EDGE ( 'NONE', *, *, #8730, .F. ) ;
#3435 = EDGE_LOOP ( 'NONE', ( #15644, #22881, #10435, #22509 ) ) ;
#3436 = AXIS2_PLACEMENT_3D ( 'NONE', #22401, #21132, #10341 ) ;
#3437 = AXIS2_PLACEMENT_3D ( 'NONE', #9950, #18739, #5888 ) ;
#3438 = CARTESIAN_POINT ( 'NONE',  ( 123.3932000000010021, -3670.300000000000182, 2260.600000000000364 ) ) ;
#3439 = ORIENTED_EDGE ( 'NONE', *, *, #20177, .F. ) ;
#3440 = EDGE_LOOP ( 'NONE', ( #3392, #17178, #6717, #10395 ) ) ;
#3441 = CARTESIAN_POINT ( 'NONE',  ( 142.5447999999993272, -3659.956214629431543, 2256.063560000000962 ) ) ;
#3442 = DATE_TIME_ROLE ( 'classification_date' ) ;
#3443 = DIRECTION ( 'NONE',  ( 0.000000000000000000, 0.000000000000000000, -1.000000000000000000 ) ) ;
#3444 = CARTESIAN_POINT ( 'NONE',  ( -6.730999999999872863, -3660.140000000000327, 2252.853000000000065 ) ) ;
#3445 = ORIENTED_EDGE ( 'NONE', *, *, #333, .T. ) ;
#3446 = DIRECTION ( 'NONE',  ( 0.000000000000000000, 0.000000000000000000, 1.000000000000000000 ) ) ;
#3447 = FACE_BOUND ( 'NONE', #19442, .T. ) ;
#3448 = CARTESIAN_POINT ( 'NONE',  ( -6.349999999999999645, -3660.140000000000327, 2247.392000000000280 ) ) ;
#3449 = DIRECTION ( 'NONE',  ( 0.000000000000000000, 0.000000000000000000, -1.000000000000000000 ) ) ;
#3450 = AXIS2_PLACEMENT_3D ( 'NONE', #4410, #9682, #6296 ) ;
#3451 = ORIENTED_EDGE ( 'NONE', *, *, #6945, .F. ) ;
#3452 = PERSON_AND_ORGANIZATION_ROLE ( 'design_supplier' ) ;
#3453 = CARTESIAN_POINT ( 'NONE',  ( 131.8035393939117341, -3543.438513001066440, 2259.907745842177974 ) ) ;
#3454 = CIRCLE ( 'NONE', #2694, 2.844800000000091700 ) ;
#3455 = CIRCLE ( 'NONE', #8332, 6.349999999999855760 ) ;
#3456 = FACE_OUTER_BOUND ( 'NONE', #385, .T. ) ;
#3457 = DIRECTION ( 'NONE',  ( 0.000000000000000000, 0.000000000000000000, -1.000000000000000000 ) ) ;
#3458 = VERTEX_POINT ( 'NONE', #17882 ) ;
#3459 = FACE_BOUND ( 'NONE', #1750, .T. ) ;
#3460 = DIRECTION ( 'NONE',  ( -1.000000000000000000, 0.000000000000000000, 0.000000000000000000 ) ) ;
#3461 = DIRECTION ( 'NONE',  ( -0.000000000000000000, 1.000000000000000000, 0.000000000000000000 ) ) ;
#3462 = DIRECTION ( 'NONE',  ( 0.000000000000000000, -1.000000000000000000, 0.000000000000000000 ) ) ;
#3463 = AXIS2_PLACEMENT_3D ( 'NONE', #9873, #13279, #18444 ) ;
#3464 = CARTESIAN_POINT ( 'NONE',  ( 9.926995637850000165, -3660.140002548000211, 2250.236801297000056 ) ) ;
#3465 = DIRECTION ( 'NONE',  ( 0.000000000000000000, 0.000000000000000000, 1.000000000000000000 ) ) ;
#3466 = ORIENTED_EDGE ( 'NONE', *, *, #6267, .F. ) ;
#3467 = VECTOR ( 'NONE', #10156, 1000.000000000000000 ) ;
#3468 = CARTESIAN_POINT ( 'NONE',  ( 12.69999999997359019, -3636.810099999929662, 2296.210799999999836 ) ) ;
#3469 = PRODUCT_DEFINITION ( 'UNKNOWN', '', #16085, #8320 ) ;
#3470 = AXIS2_PLACEMENT_3D ( 'NONE', #19594, #22977, #14209 ) ;
#3471 = DIRECTION ( 'NONE',  ( 0.000000000000000000, -1.000000000000000000, 0.000000000000000000 ) ) ;
#3472 = CARTESIAN_POINT ( 'NONE',  ( 15.00430973647434207, -3657.836720156582942, 2249.062018686695865 ) ) ;
#3473 = CARTESIAN_POINT ( 'NONE',  ( 137.0287870094147422, -3695.282573428062278, 2255.445345400565202 ) ) ;
#3474 = CARTESIAN_POINT ( 'NONE',  ( 10.37685559933697554, -3577.852505989571910, 2250.052669706260076 ) ) ;
#3475 = ORIENTED_EDGE ( 'NONE', *, *, #19626, .F. ) ;
#3476 = EDGE_CURVE ( 'NONE', #9977, #19601, #23081, .T. ) ;
#3477 = CARTESIAN_POINT ( 'NONE',  ( 132.2768405780999785, -3544.527728670999750, 2260.413001451000127 ) ) ;
#3478 = EDGE_CURVE ( 'NONE', #14198, #5385, #10364, .T. ) ;
#3479 = DIRECTION ( 'NONE',  ( -1.000000000000000000, 0.000000000000000000, 0.000000000000000000 ) ) ;
#3481 = VECTOR ( 'NONE', #14074, 1000.000000000000000 ) ;
#3480 = PERSON_AND_ORGANIZATION_ROLE ( 'classification_officer' ) ;
#3482 = EDGE_CURVE ( 'NONE', #19496, #3614, #18592, .T. ) ;
#3483 = PLANE ( 'NONE',  #7214 ) ;
#3484 = DIRECTION ( 'NONE',  ( -1.000000000000000000, 0.000000000000000000, 0.000000000000000000 ) ) ;
#3485 = CARTESIAN_POINT ( 'NONE',  ( 20.09942059832000183, -3694.430000000000291, 2260.390449568000349 ) ) ;
#3486 = AXIS2_PLACEMENT_3D ( 'NONE', #9986, #22396, #11398 ) ;
#3487 = CYLINDRICAL_SURFACE ( 'NONE', #16375, 1.269999999999898099 ) ;
#3488 = DIRECTION ( 'NONE',  ( -0.7249994335945011414, 0.000000000000000000, 0.6887494619146010688 ) ) ;
#3489 = CLOSED_SHELL ( 'NONE', ( #15133, #15720, #807, #10568, #14427, #9706, #6724, #8142, #12688, #11075, #12372, #1399, #697, #20814, #10739, #8144, #11809, #12080, #21605, #11371, #23130, #1468, #22244, #13702, #17948, #11438 ) ) ;
#3490 = EDGE_CURVE ( 'NONE', #12180, #2780, #1380, .T. ) ;
#3491 = EDGE_LOOP ( 'NONE', ( #17907, #11275 ) ) ;
#3492 = CARTESIAN_POINT ( 'NONE',  ( 10.36831320292846925, -3580.841200000038953, 2239.391000000000076 ) ) ;
#3493 = CARTESIAN_POINT ( 'NONE',  ( 18.41499999999999915, -3659.504999999999654, 2246.630000000000109 ) ) ;
#3494 = ORIENTED_EDGE ( 'NONE', *, *, #19752, .F. ) ;
#3495 = CARTESIAN_POINT ( 'NONE',  ( -5.588000000000000078, -3544.061999999999898, 2254.250000000000000 ) ) ;
#3496 = AXIS2_PLACEMENT_3D ( 'NONE', #21078, #13929, #10635 ) ;
#3497 = ORIENTED_EDGE ( 'NONE', *, *, #5585, .T. ) ;
#3498 = CARTESIAN_POINT ( 'NONE',  ( -12.31900000000000084, -3578.860000000000127, 2250.104686796999886 ) ) ;
#3499 = CARTESIAN_POINT ( 'NONE',  ( 142.5447969220999767, -3659.599750067000059, 2250.186720660999981 ) ) ;
#3500 = ORIENTED_EDGE ( 'NONE', *, *, #1628, .T. ) ;
#3501 = CIRCLE ( 'NONE', #20712, 6.349999999999855760 ) ;
#3502 = ADVANCED_FACE ( 'NONE', ( #528 ), #10736, .F. ) ;
#3503 = CARTESIAN_POINT ( 'NONE',  ( 136.8708886487836480, -3579.840085227391228, 2250.069118183399041 ) ) ;
#3504 = EDGE_CURVE ( 'NONE', #16691, #10464, #22326, .T. ) ;
#3505 = ORIENTED_EDGE ( 'NONE', *, *, #9833, .T. ) ;
#3506 = CARTESIAN_POINT ( 'NONE',  ( 145.4149999194000316, -3579.495498070999474, 2244.618783703000190 ) ) ;
#3507 = ADVANCED_FACE ( 'NONE', ( #11192 ), #1827, .T. ) ;
#3508 = APPROVAL_STATUS ( 'not_yet_approved' ) ;
#3509 = EDGE_CURVE ( 'NONE', #1092, #8539, #3621, .T. ) ;
#3510 = FACE_OUTER_BOUND ( 'NONE', #13026, .T. ) ;
#3511 = CARTESIAN_POINT ( 'NONE',  ( 139.6999999999999886, -3659.504999999999654, 2246.630000000000109 ) ) ;
#3512 = CIRCLE ( 'NONE', #10626, 2.844800000000091700 ) ;
#3513 = CARTESIAN_POINT ( 'NONE',  ( 0.000000000000000000, -3544.061999999999898, 2239.771999999999935 ) ) ;
#3514 = DIRECTION ( 'NONE',  ( 0.000000000000000000, -1.000000000000000000, 0.000000000000000000 ) ) ;
#3515 = EDGE_LOOP ( 'NONE', ( #14355, #15325, #10772, #722, #20412, #21842, #22936, #4256, #6040 ) ) ;
#3516 = FACE_OUTER_BOUND ( 'NONE', #12231, .T. ) ;
#3517 = DIRECTION ( 'NONE',  ( 0.000000000000000000, 0.000000000000000000, -1.000000000000000000 ) ) ;
#3518 = VERTEX_POINT ( 'NONE', #1945 ) ;
#3519 = CARTESIAN_POINT ( 'NONE',  ( 5.080000000000000071, -3694.746619019253558, 2260.599999999999454 ) ) ;
#3520 = DIRECTION ( 'NONE',  ( 0.7249994335944036639, 0.000000000000000000, 0.6887494619147036534 ) ) ;
#3521 = FACE_OUTER_BOUND ( 'NONE', #17562, .T. ) ;
#3522 = ORIENTED_EDGE ( 'NONE', *, *, #5424, .T. ) ;
#3523 = CARTESIAN_POINT ( 'NONE',  ( 12.69999999999999929, -3639.502500000000055, 2263.571799999999712 ) ) ;
#3524 = CARTESIAN_POINT ( 'NONE',  ( 12.69999999999999929, -3653.027999999999793, 2268.705139999999574 ) ) ;
#3525 = AXIS2_PLACEMENT_3D ( 'NONE', #18593, #9791, #11657 ) ;
#3526 = VERTEX_POINT ( 'NONE', #19874 ) ;
#3527 = CIRCLE ( 'NONE', #4664, 4.114799999999974034 ) ;
#3528 = DIRECTION ( 'NONE',  ( 0.8660254037825247941, 0.5000000000033149039, 0.000000000000000000 ) ) ;
#3529 = CARTESIAN_POINT ( 'NONE',  ( 9.855201422231997910, -3639.607849033000093, 2279.447341858000073 ) ) ;
#3530 = AXIS2_PLACEMENT_3D ( 'NONE', #13526, #9774, #11758 ) ;
#3531 = DIRECTION ( 'NONE',  ( 0.000000000000000000, 0.000000000000000000, -1.000000000000000000 ) ) ;
#3532 = UNCERTAINTY_MEASURE_WITH_UNIT (LENGTH_MEASURE( 1.000000000000000082E-05 ), #4715, 'distance_accuracy_value', 'NONE');
#3533 = APPROVAL_STATUS ( 'not_yet_approved' ) ;
#3534 = ORIENTED_EDGE ( 'NONE', *, *, #9315, .F. ) ;
#3535 = CARTESIAN_POINT ( 'NONE',  ( 12.69999999999999929, -3601.402499999999691, 2263.571799999999712 ) ) ;
#3536 = DIRECTION ( 'NONE',  ( 1.000000000000000000, 0.000000000000000000, 0.000000000000000000 ) ) ;
#3537 = ORIENTED_EDGE ( 'NONE', *, *, #6592, .F. ) ;
#3538 = CARTESIAN_POINT ( 'NONE',  ( 147.8270794805000037, -3695.699999999999818, 2259.329999999999927 ) ) ;
#3539 = ADVANCED_FACE ( 'NONE', ( #9095 ), #7560, .F. ) ;
#3540 = CARTESIAN_POINT ( 'NONE',  ( 136.9819489059368323, -3658.646220300227014, 2249.821879689220168 ) ) ;
#3541 = EDGE_CURVE ( 'NONE', #12671, #15650, #21955, .T. ) ;
#3542 = CIRCLE ( 'NONE', #2488, 4.114799999999974034 ) ;
#3543 = ORIENTED_EDGE ( 'NONE', *, *, #7244, .F. ) ;
#3544 = AXIS2_PLACEMENT_3D ( 'NONE', #9275, #16407, #21687 ) ;
#3545 = CARTESIAN_POINT ( 'NONE',  ( 34.49320000000000164, -3644.899999999999636, 2260.600000000000364 ) ) ;
#3546 = AXIS2_PLACEMENT_3D ( 'NONE', #7593, #16496, #1861 ) ;
#3547 = ORIENTED_EDGE ( 'NONE', *, *, #2009, .T. ) ;
#3548 = AXIS2_PLACEMENT_3D ( 'NONE', #7777, #13494, #15149 ) ;
#3549 = ORIENTED_EDGE ( 'NONE', *, *, #17653, .F. ) ;
#3550 = ADVANCED_FACE ( 'NONE', ( #10962 ), #9212, .F. ) ;
#3551 = ORIENTED_EDGE ( 'NONE', *, *, #8136, .T. ) ;
#3552 = DIRECTION ( 'NONE',  ( 0.000000000000000000, 0.000000000000000000, -1.000000000000000000 ) ) ;
#3553 = ORIENTED_EDGE ( 'NONE', *, *, #8384, .T. ) ;
#3554 = ORIENTED_EDGE ( 'NONE', *, *, #8673, .T. ) ;
#3555 = DIRECTION ( 'NONE',  ( 1.000000000000000000, -2.334777064353000131E-14, -2.343004830739999973E-14 ) ) ;
#3556 = DATE_AND_TIME ( #9072, #8656 ) ;
#3557 = CARTESIAN_POINT ( 'NONE',  ( 142.4126867972000241, -3579.494999999999891, 2239.391000000000076 ) ) ;
#3558 = DIRECTION ( 'NONE',  ( 1.000000000000000000, 0.000000000000000000, 0.000000000000000000 ) ) ;
#3559 = ADVANCED_FACE ( 'NONE', ( #2183 ), #21606, .T. ) ;
#3560 = ORIENTED_EDGE ( 'NONE', *, *, #12253, .F. ) ;
#3561 = LINE ( 'NONE', #14239, #21212 ) ;
#3562 = EDGE_CURVE ( 'NONE', #8027, #9982, #6264, .T. ) ;
#3563 = FACE_BOUND ( 'NONE', #14863, .T. ) ;
#3564 = AXIS2_PLACEMENT_3D ( 'NONE', #9359, #7826, #22111 ) ;
#3565 = B_SPLINE_CURVE_WITH_KNOTS ( 'NONE', 3,
 ( #7621, #22339, #14781, #1128 ),
 .UNSPECIFIED., .F., .F.,
 ( 4, 4 ),
 ( 0.000000000000000000, 1.000000000000000000 ),
 .UNSPECIFIED. ) ;
#3566 = AXIS2_PLACEMENT_3D ( 'NONE', #12523, #19671, #1746 ) ;
#3567 = DIRECTION ( 'NONE',  ( 0.000000000000000000, -1.000000000000000000, -2.848874176402999842E-12 ) ) ;
#3568 = PERSON_AND_ORGANIZATION ( #5446, #1895 ) ;
#3569 = VECTOR ( 'NONE', #2654, 1000.000000000000000 ) ;
#3570 = AXIS2_PLACEMENT_3D ( 'NONE', #22507, #17348, #10448 ) ;
#3571 = DIRECTION ( 'NONE',  ( 0.000000000000000000, 0.000000000000000000, -1.000000000000000000 ) ) ;
#3572 = CARTESIAN_POINT ( 'NONE',  ( 18.16100000000000136, -3579.494999999999891, 2239.391000000000076 ) ) ;
#3573 = EDGE_CURVE ( 'NONE', #8067, #20661, #18227, .T. ) ;
#3574 = DIRECTION ( 'NONE',  ( 1.000000000000000000, 0.000000000000000000, 0.000000000000000000 ) ) ;
#3575 = ORIENTED_EDGE ( 'NONE', *, *, #4783, .T. ) ;
#3576 = DIRECTION ( 'NONE',  ( 1.000000000000000000, 0.000000000000000000, 0.000000000000000000 ) ) ;
#3577 = VECTOR ( 'NONE', #13440, 1000.000000000000227 ) ;
#3578 = CARTESIAN_POINT ( 'NONE',  ( 10.16000000000000014, -3660.786127253999894, 2255.774000000000342 ) ) ;
#3579 = DIRECTION ( 'NONE',  ( 0.000000000000000000, 0.000000000000000000, 1.000000000000000000 ) ) ;
#3580 = CYLINDRICAL_SURFACE ( 'NONE', #7749, 2.844800000000091700 ) ;
#3581 = CIRCLE ( 'NONE', #22655, 5.460999999999938126 ) ;
#3582 = CYLINDRICAL_SURFACE ( 'NONE', #13634, 2.844800000000001550 ) ;
#3583 = CIRCLE ( 'NONE', #7341, 0.3809999999999647002 ) ;
#3584 = CARTESIAN_POINT ( 'NONE',  ( 147.5628652634462128, -3543.485052021266711, 2259.991528816362461 ) ) ;
#3585 = AXIS2_PLACEMENT_3D ( 'NONE', #19438, #20849, #13821 ) ;
#3586 = EDGE_LOOP ( 'NONE', ( #10181, #18085, #6846, #6850 ) ) ;
#3587 = FACE_OUTER_BOUND ( 'NONE', #8459, .T. ) ;
#3588 = VECTOR ( 'NONE', #1643, 1000.000000000000000 ) ;
#3589 = FACE_OUTER_BOUND ( 'NONE', #3274, .T. ) ;
#3590 = DIRECTION ( 'NONE',  ( 0.000000000000000000, 0.000000000000000000, 1.000000000000000000 ) ) ;
#3591 = CARTESIAN_POINT ( 'NONE',  ( 14.60426581554083825, -3657.391551304373479, 2248.126455225663904 ) ) ;
#3592 = LINE ( 'NONE', #10747, #13559 ) ;
#3593 = DIRECTION ( 'NONE',  ( 0.000000000000000000, 0.000000000000000000, -1.000000000000000000 ) ) ;
#3594 = EDGE_LOOP ( 'NONE', ( #12986, #3899, #22604, #15326 ) ) ;
#3595 = VECTOR ( 'NONE', #1333, 1000.000000000000000 ) ;
#3596 = CARTESIAN_POINT ( 'NONE',  ( 10.01417881486321271, -3543.678681369438891, 2255.408746714403605 ) ) ;
#3597 = AXIS2_PLACEMENT_3D ( 'NONE', #21374, #11174, #18313 ) ;
#3598 = PERSON_AND_ORGANIZATION ( #12997, #4153 ) ;
#3599 = DIRECTION ( 'NONE',  ( 0.000000000000000000, 0.000000000000000000, 1.000000000000000000 ) ) ;
#3600 = AXIS2_PLACEMENT_3D ( 'NONE', #2794, #8079, #13462 ) ;
#3601 = DIRECTION ( 'NONE',  ( -0.7249994335945011414, -6.625572310377011455E-14, -0.6887494619146010688 ) ) ;
#3602 = AXIS2_PLACEMENT_3D ( 'NONE', #10731, #12488, #1706 ) ;
#3603 = DIRECTION ( 'NONE',  ( 0.000000000000000000, -1.000000000000000000, 0.000000000000000000 ) ) ;
#3604 = APPROVAL ( #9023, 'UNSPECIFIED' ) ;
#3605 = VERTEX_POINT ( 'NONE', #18224 ) ;
#3606 = CARTESIAN_POINT ( 'NONE',  ( 12.70000020906999971, -3582.339800010000090, 2257.592639999999847 ) ) ;
#3607 = VERTEX_POINT ( 'NONE', #9328 ) ;
#3608 = DIRECTION ( 'NONE',  ( 0.000000000000000000, 0.000000000000000000, -1.000000000000000000 ) ) ;
#3609 = EDGE_CURVE ( 'NONE', #10134, #22010, #18608, .T. ) ;
#3610 = FACE_OUTER_BOUND ( 'NONE', #16005, .T. ) ;
#3611 = VERTEX_POINT ( 'NONE', #5934 ) ;
#3612 = DIRECTION ( 'NONE',  ( 0.000000000000000000, 0.000000000000000000, 1.000000000000000000 ) ) ;
#3613 = AXIS2_PLACEMENT_3D ( 'NONE', #17482, #17597, #8703 ) ;
#3614 = VERTEX_POINT ( 'NONE', #21705 ) ;
#3615 = CARTESIAN_POINT ( 'NONE',  ( 137.3683132029851208, -3580.841200000048957, 2239.391000000000076 ) ) ;
#3616 = FACE_OUTER_BOUND ( 'NONE', #20784, .T. ) ;
#3617 = AXIS2_PLACEMENT_3D ( 'NONE', #6325, #8424, #12168 ) ;
#3618 = AXIS2_PLACEMENT_3D ( 'NONE', #18906, #17025, #2617 ) ;
#3619 = ORIENTED_EDGE ( 'NONE', *, *, #2676, .T. ) ;
#3620 = VERTEX_POINT ( 'NONE', #10806 ) ;
#3621 = CIRCLE ( 'NONE', #1003, 5.080000000000000959 ) ;
#3622 = CARTESIAN_POINT ( 'NONE',  ( 137.5384828158008759, -3581.344674309946186, 2248.777575039056501 ) ) ;
#3623 = ORIENTED_EDGE ( 'NONE', *, *, #15602, .T. ) ;
#3624 = DIRECTION ( 'NONE',  ( -1.000000000000000000, -2.186138625658999988E-13, 0.000000000000000000 ) ) ;
#3625 = PERSON_AND_ORGANIZATION_ROLE ( 'design_supplier' ) ;
#3626 = CARTESIAN_POINT ( 'NONE',  ( 151.4000000000000057, -3694.430000000000291, 2240.279999999999745 ) ) ;
#3627 = CARTESIAN_POINT ( 'NONE',  ( -0.7620000000000000107, -3544.061999999999898, 2254.250000000000000 ) ) ;
#3628 = VECTOR ( 'NONE', #14541, 1000.000000000000000 ) ;
#3629 = APPLIED_PERSON_AND_ORGANIZATION_ASSIGNMENT ( #10836, #7326, ( #6402 ) ) ;
#3630 = CARTESIAN_POINT ( 'NONE',  ( 12.69999999999999929, -3648.710000000000036, 2268.705139999999574 ) ) ;
#3631 = AXIS2_PLACEMENT_3D ( 'NONE', #21475, #13136, #9733 ) ;
#3632 = CARTESIAN_POINT ( 'NONE',  ( 64.76999999999999602, -3694.938000000000102, 2289.213099999999940 ) ) ;
#3633 = ORIENTED_EDGE ( 'NONE', *, *, #12507, .F. ) ;
#3634 = CARTESIAN_POINT ( 'NONE',  ( 134.8493656935452520, -3576.472980476652083, 2245.844349661984779 ) ) ;
#3635 = CIRCLE ( 'NONE', #12262, 2.844799999999994444 ) ;
#3636 = EDGE_CURVE ( 'NONE', #3840, #22617, #17949, .T. ) ;
#3637 = CIRCLE ( 'NONE', #1772, 0.7619999999999294005 ) ;
#3638 = CARTESIAN_POINT ( 'NONE',  ( 61.26424768829000556, -3544.061999999999898, 2279.827800000000025 ) ) ;
#3639 = VERTEX_POINT ( 'NONE', #3535 ) ;
#3640 = EDGE_CURVE ( 'NONE', #1044, #18165, #20483, .T. ) ;
#3641 = CYLINDRICAL_SURFACE ( 'NONE', #21140, 0.3809999999999121312 ) ;
#3642 = DIRECTION ( 'NONE',  ( 0.000000000000000000, 0.000000000000000000, -1.000000000000000000 ) ) ;
#3643 = EDGE_CURVE ( 'NONE', #2024, #13470, #22490, .T. ) ;
#3644 = DIRECTION ( 'NONE',  ( 0.000000000000000000, 0.000000000000000000, 1.000000000000000000 ) ) ;
#3645 = EDGE_LOOP ( 'NONE', ( #13445, #11800, #11607, #22995 ) ) ;
#3646 = CARTESIAN_POINT ( 'NONE',  ( 12.79204376678999999, -3662.349799990000065, 2257.592639999999847 ) ) ;
#3647 = CYLINDRICAL_SURFACE ( 'NONE', #8054, 2.844800000000091700 ) ;
#3648 = ORIENTED_EDGE ( 'NONE', *, *, #2579, .F. ) ;
#3649 = AXIS2_PLACEMENT_3D ( 'NONE', #18715, #13220, #7729 ) ;
#3650 = CARTESIAN_POINT ( 'NONE',  ( 12.69999999999999929, -3590.289999999999964, 2268.705139999999574 ) ) ;
#3651 = CARTESIAN_POINT ( 'NONE',  ( 12.69999999999999929, -3655.060000000000400, 2268.705139999999574 ) ) ;
#3652 = FACE_OUTER_BOUND ( 'NONE', #13773, .T. ) ;
#3653 = DIRECTION ( 'NONE',  ( 0.000000000000000000, 1.000000000000000000, 0.000000000000000000 ) ) ;
#3654 = APPROVAL_DATE_TIME ( #19830, #14222 ) ;
#3655 = AXIS2_PLACEMENT_3D ( 'NONE', #13280, #4267, #13403 ) ;
#3656 = DIRECTION ( 'NONE',  ( 0.000000000000000000, -1.000000000000000000, 0.000000000000000000 ) ) ;
#3657 = CARTESIAN_POINT ( 'NONE',  ( 129.8447999999989975, -3670.300000000000182, 2259.837999999999738 ) ) ;
#3658 = ORIENTED_EDGE ( 'NONE', *, *, #9433, .F. ) ;
#3659 = CARTESIAN_POINT ( 'NONE',  ( 12.69999999999999929, -3639.502500000000055, 2288.971800000000258 ) ) ;
#3660 = ADVANCED_FACE ( 'NONE', ( #19602 ), #21362, .T. ) ;
#3661 = CARTESIAN_POINT ( 'NONE',  ( 137.7873330486999919, -3657.399152860999493, 2246.630000000000109 ) ) ;
#3662 = EDGE_LOOP ( 'NONE', ( #14176, #11005 ) ) ;
#3663 = B_SPLINE_CURVE_WITH_KNOTS ( 'NONE', 3,
 ( #3114, #1710, #8629, #1357, #22790, #7110 ),
 .UNSPECIFIED., .F., .F.,
 ( 4, 1, 1, 4 ),
 ( 0.000000000000000000, 0.3333333333333000081, 0.6666666666667000474, 1.000000000000000000 ),
 .UNSPECIFIED. ) ;
#3664 = ORIENTED_EDGE ( 'NONE', *, *, #2084, .F. ) ;
#3665 = CARTESIAN_POINT ( 'NONE',  ( 137.5048382467581973, -3661.314614866817010, 2249.983038987777491 ) ) ;
#3666 = CIRCLE ( 'NONE', #11170, 5.460999999999938126 ) ;
#3667 = ORIENTED_EDGE ( 'NONE', *, *, #1191, .F. ) ;
#3668 = ORIENTED_EDGE ( 'NONE', *, *, #7698, .T. ) ;
#3669 = VERTEX_POINT ( 'NONE', #15854 ) ;
#3670 = EDGE_CURVE ( 'NONE', #7352, #11125, #6644, .T. ) ;
#3671 = VERTEX_POINT ( 'NONE', #9050 ) ;
#3672 = EDGE_LOOP ( 'NONE', ( #21112, #2496 ) ) ;
#3673 = PLANE ( 'NONE',  #21747 ) ;
#3674 = COORDINATED_UNIVERSAL_TIME_OFFSET ( 0, 0, .AHEAD. ) ;
#3675 = CARTESIAN_POINT ( 'NONE',  ( 0.7620000000000000107, -3694.938000000000102, 2296.591799999999694 ) ) ;
#3676 = FACE_OUTER_BOUND ( 'NONE', #2813, .T. ) ;
#3677 = EDGE_CURVE ( 'NONE', #21672, #10931, #1790, .T. ) ;
#3678 = ORIENTED_EDGE ( 'NONE', *, *, #13410, .T. ) ;
#3679 = ADVANCED_FACE ( 'NONE', ( #8821 ), #8517, .T. ) ;
#3680 = CARTESIAN_POINT ( 'NONE',  ( 1.270000000000000018, -3694.430000000000291, 2239.009999999999764 ) ) ;
#3681 = FACE_OUTER_BOUND ( 'NONE', #2689, .T. ) ;
#3682 = CARTESIAN_POINT ( 'NONE',  ( 7.387125747139000609, -3581.600847139000052, 2246.630000000000109 ) ) ;
#3683 = DIRECTION ( 'NONE',  ( 0.000000000000000000, 1.000000000000000000, 0.000000000000000000 ) ) ;
#3684 = CALENDAR_DATE ( 2026, 26, 10 ) ;
#3685 = VERTEX_POINT ( 'NONE', #33 ) ;
#3686 = CARTESIAN_POINT ( 'NONE',  ( 131.7910775263680705, -3543.423052263211048, 2259.876519366634511 ) ) ;
#3687 = VERTEX_POINT ( 'NONE', #18070 ) ;
#3688 = DIRECTION ( 'NONE',  ( 0.000000000000000000, -1.000000000000000000, 0.000000000000000000 ) ) ;
#3689 = CARTESIAN_POINT ( 'NONE',  ( 151.4000000000000057, -3694.938000000000102, 2279.827800000000025 ) ) ;
#3690 = ORIENTED_EDGE ( 'NONE', *, *, #12800, .T. ) ;
#3691 = ADVANCED_FACE ( 'NONE', ( #151 ), #7297, .F. ) ;
#3692 = FACE_OUTER_BOUND ( 'NONE', #7113, .T. ) ;
#3693 = DIRECTION ( 'NONE',  ( 0.000000000000000000, -2.336881798971000105E-14, -1.000000000000000000 ) ) ;
#3694 = CARTESIAN_POINT ( 'NONE',  ( 145.3474457849973192, -3578.572730242030048, 2244.547227117760031 ) ) ;
#3695 = DIRECTION ( 'NONE',  ( 0.000000000000000000, 0.000000000000000000, -1.000000000000000000 ) ) ;
#3696 = DIRECTION ( 'NONE',  ( 0.000000000000000000, 0.000000000000000000, -1.000000000000000000 ) ) ;
#3697 = CARTESIAN_POINT ( 'NONE',  ( 147.5856715291725720, -3543.452888078975775, 2259.934476224082118 ) ) ;
#3698 = ORIENTED_EDGE ( 'NONE', *, *, #2383, .T. ) ;
#3699 = DIRECTION ( 'NONE',  ( -0.000000000000000000, 1.000000000000000000, 0.000000000000000000 ) ) ;
#3700 = VECTOR ( 'NONE', #8059, 1000.000000000000000 ) ;
#3701 = CARTESIAN_POINT ( 'NONE',  ( 151.4000000000000057, -3660.140000000000327, 2244.518167364599321 ) ) ;
#3702 = ADVANCED_FACE ( 'NONE', ( #14214 ), #11038, .T. ) ;
#3703 = FACE_OUTER_BOUND ( 'NONE', #14086, .T. ) ;
#3704 = CARTESIAN_POINT ( 'NONE',  ( 142.4278116317892113, -3543.579977979913565, 2255.303812752575141 ) ) ;
#3705 = DIRECTION ( 'NONE',  ( 1.224646799147353207E-16, 1.000000000000000000, -0.000000000000000000 ) ) ;
#3706 = CARTESIAN_POINT ( 'NONE',  ( 7.700590725981468765, -3576.724945326997840, 2245.509351448440157 ) ) ;
#3707 = ORIENTED_EDGE ( 'NONE', *, *, #17142, .F. ) ;
#3708 = DIRECTION ( 'NONE',  ( 0.000000000000000000, 0.000000000000000000, 1.000000000000000000 ) ) ;
#3709 = DIRECTION ( 'NONE',  ( 1.122008997397786234E-13, 0.000000000000000000, 1.000000000000000000 ) ) ;
#3710 = ITEM_DEFINED_TRANSFORMATION ( 'NONE', 'NONE', #10101,  #5611 ) ;
#3711 = AXIS2_PLACEMENT_3D ( 'NONE', #766, #20463, #4411 ) ;
#3712 = CARTESIAN_POINT ( 'NONE',  ( 12.69999999999999929, -3634.041499999999814, 2290.622800000000097 ) ) ;
#3713 = CARTESIAN_POINT ( 'NONE',  ( 0.000000000000000000, -3660.140000000000327, 2243.785200000000259 ) ) ;
#3714 = CARTESIAN_POINT ( 'NONE',  ( 0.000000000000000000, -3694.938000000000102, 2253.487999999999829 ) ) ;
#3715 = CIRCLE ( 'NONE', #16809, 0.7619999999999294005 ) ;
#3716 = ADVANCED_FACE ( 'NONE', ( #12334 ), #5553, .T. ) ;
#3717 = EDGE_CURVE ( 'NONE', #13767, #7858, #8705, .T. ) ;
#3718 = DIRECTION ( 'NONE',  ( -1.000000000000000000, 0.000000000000000000, 0.000000000000000000 ) ) ;
#3719 = CARTESIAN_POINT ( 'NONE',  ( -5.588000000000000078, -3660.140000000000327, 2247.392000000000280 ) ) ;
#3720 = ORIENTED_EDGE ( 'NONE', *, *, #3134, .F. ) ;
#3721 = DIRECTION ( 'NONE',  ( 1.000000000000000000, 0.000000000000000000, 0.000000000000000000 ) ) ;
#3722 = CARTESIAN_POINT ( 'NONE',  ( 10.00572897464999933, -3638.571071898999890, 2279.486249620000308 ) ) ;
#3723 = ORIENTED_EDGE ( 'NONE', *, *, #4779, .T. ) ;
#3724 = DIRECTION ( 'NONE',  ( 0.000000000000000000, 0.000000000000000000, 1.000000000000000000 ) ) ;
#3725 = B_SPLINE_CURVE_WITH_KNOTS ( 'NONE', 3,
 ( #34, #17601, #12685, #14215, #18071, #152, #21598, #12568, #5310, #9173, #274, #1552, #8706, #22984, #19603, #16314, #15855, #7298, #7074, #6956, #14100, #10807, #8938, #14451 ),
 .UNSPECIFIED., .F., .F.,
 ( 4, 2, 2, 1, 1, 1, 2, 2, 2, 2, 1, 2, 2, 4 ),
 ( 0.000000000000000000, 0.1249999999958202324, 0.1874999999936646511, 0.2187499999925868743, 0.2343749999925359984, 0.2421874999925105743, 0.2460937499923391558, 0.2499999999921677096, 0.3749999999942763562, 0.4374999999955747620, 0.4687499999961892705, 0.4843749999962707609, 0.4999999999963522512, 1.000000000000000000 ),
 .UNSPECIFIED. ) ;
#3726 = VECTOR ( 'NONE', #14539, 1000.000000000000000 ) ;
#3727 = ORIENTED_EDGE ( 'NONE', *, *, #12607, .T. ) ;
#3728 = CARTESIAN_POINT ( 'NONE',  ( 25.39999999999999858, -3619.500000000000000, 2259.837999999999738 ) ) ;
#3729 = CARTESIAN_POINT ( 'NONE',  ( 1.270000000000000018, -3660.140000000000327, 2247.392000000000280 ) ) ;
#3730 = PRODUCT_DEFINITION_FORMATION_WITH_SPECIFIED_SOURCE ( 'ANY', '', #7149, .NOT_KNOWN. ) ;
#3731 = CIRCLE ( 'NONE', #21691, 1.269999999999882334 ) ;
#3732 = ORIENTED_EDGE ( 'NONE', *, *, #1841, .T. ) ;
#3733 = ORIENTED_EDGE ( 'NONE', *, *, #15826, .T. ) ;
#3734 = CARTESIAN_POINT ( 'NONE',  ( 137.4641237087990930, -3581.254761593761941, 2248.929472245830311 ) ) ;
#3735 = VERTEX_POINT ( 'NONE', #19484 ) ;
#3736 = DIRECTION ( 'NONE',  ( 0.000000000000000000, -1.000000000000000000, 0.000000000000000000 ) ) ;
#3737 = CALENDAR_DATE ( 2026, 26, 10 ) ;
#3738 = CARTESIAN_POINT ( 'NONE',  ( 92.50679999999999836, -3594.099999999999909, 2260.600000000000364 ) ) ;
#3739 = LINE ( 'NONE', #3863, #18974 ) ;
#3740 = LINE ( 'NONE', #3864, #7779 ) ;
#3741 = CARTESIAN_POINT ( 'NONE',  ( 61.26424768829000556, -3694.938000000000102, 2279.827800000000025 ) ) ;
#3742 = LOCAL_TIME ( 17, 37, 43.00000000000000000, #790 ) ;
#3743 = CARTESIAN_POINT ( 'NONE',  ( 140.5358672174552339, -3576.775707768860229, 2249.328148595326638 ) ) ;
#3744 = ORIENTED_EDGE ( 'NONE', *, *, #3430, .F. ) ;
#3745 = CARTESIAN_POINT ( 'NONE',  ( 134.7245833821262977, -3576.682656229064833, 2245.560154887602948 ) ) ;
#3746 = CARTESIAN_POINT ( 'NONE',  ( 101.5999999999999943, -3670.300000000000182, 2239.771999999999935 ) ) ;
#3747 = AXIS2_PLACEMENT_3D ( 'NONE', #11032, #16309, #266 ) ;
#3748 = ORIENTED_EDGE ( 'NONE', *, *, #17860, .T. ) ;
#3749 = CARTESIAN_POINT ( 'NONE',  ( 0.000000000000000000, -3694.938000000000102, 2275.763800000000174 ) ) ;
#3750 = LINE ( 'NONE', #9038, #7618 ) ;
#3751 = EDGE_LOOP ( 'NONE', ( #1917, #10305, #3998, #14179 ) ) ;
#3752 = DIRECTION ( 'NONE',  ( 0.000000000000000000, 0.000000000000000000, -1.000000000000000000 ) ) ;
#3753 = DIRECTION ( 'NONE',  ( 1.000000000000000000, 0.000000000000000000, -1.224646799147353207E-16 ) ) ;
#3754 = AXIS2_PLACEMENT_3D ( 'NONE', #325, #9459, #11214 ) ;
#3755 = EDGE_LOOP ( 'NONE', ( #10231, #17493, #6970, #18639 ) ) ;
#3756 = APPLIED_DATE_AND_TIME_ASSIGNMENT ( #22062, #18212, ( #3469 ) ) ;
#3757 = DIRECTION ( 'NONE',  ( 9.814416866149999939E-14, 3.885294924330999618E-13, 1.000000000000000000 ) ) ;
#3758 = CARTESIAN_POINT ( 'NONE',  ( 10.12709285722000097, -3640.730217009000171, 2279.515989326000181 ) ) ;
#3759 = LOCAL_TIME ( 17, 37, 43.00000000000000000, #21421 ) ;
#3760 = CARTESIAN_POINT ( 'NONE',  ( 12.69999999999999929, -3579.494999999999891, 2239.391000000000076 ) ) ;
#3761 = SECURITY_CLASSIFICATION ( '', '', #4510 ) ;
#3762 = FACE_OUTER_BOUND ( 'NONE', #5461, .T. ) ;
#3763 = PERSON_AND_ORGANIZATION_ROLE ( 'design_owner' ) ;
#3764 = CIRCLE ( 'NONE', #15753, 3.175000000000149925 ) ;
#3765 = EDGE_CURVE ( 'NONE', #10812, #159, #11871, .T. ) ;
#3766 = DIRECTION ( 'NONE',  ( 0.000000000000000000, 0.000000000000000000, -1.000000000000000000 ) ) ;
#3767 = CARTESIAN_POINT ( 'NONE',  ( 15.24000000000000021, -3544.570000000000164, 2254.503999999999905 ) ) ;
#3768 = ORIENTED_EDGE ( 'NONE', *, *, #13381, .F. ) ;
#3770 = EDGE_CURVE ( 'NONE', #3611, #8104, #9631, .T. ) ;
#3769 = CYLINDRICAL_SURFACE ( 'NONE', #21280, 0.3809999999999647002 ) ;
#3771 = EDGE_CURVE ( 'NONE', #2160, #2800, #10569, .T. ) ;
#3772 = CARTESIAN_POINT ( 'NONE',  ( 137.5597418815846993, -3657.630783818591681, 2248.732918511922435 ) ) ;
#3773 = TOROIDAL_SURFACE ( 'NONE', #13144, 5.080000000000000071, 0.3810000000000000053 ) ;
#3774 = VERTEX_POINT ( 'NONE', #7522 ) ;
#3775 = CARTESIAN_POINT ( 'NONE',  ( 140.4840675020349750, -3662.239671886142332, 2249.311457353029709 ) ) ;
#3776 = EDGE_CURVE ( 'NONE', #7043, #20273, #293, .T. ) ;
#3777 = EDGE_LOOP ( 'NONE', ( #17426, #1243, #4158, #15338, #19915, #17145 ) ) ;
#3778 = LOCAL_TIME ( 17, 37, 43.00000000000000000, #17097 ) ;
#3779 = VERTEX_POINT ( 'NONE', #492 ) ;
#3780 = LINE ( 'NONE', #17853, #10301 ) ;
#3781 = ORIENTED_EDGE ( 'NONE', *, *, #15978, .F. ) ;
#3782 = ORIENTED_EDGE ( 'NONE', *, *, #14019, .F. ) ;
#3783 = DIRECTION ( 'NONE',  ( 2.324635735433000053E-14, 0.000000000000000000, 1.000000000000000000 ) ) ;
#3784 = EDGE_CURVE ( 'NONE', #8549, #13491, #20295, .T. ) ;
#3785 = CARTESIAN_POINT ( 'NONE',  ( 127.0000000000000000, -3578.860000000000127, 2250.236800000000130 ) ) ;
#3786 = CIRCLE ( 'NONE', #9421, 1.269999999999882334 ) ;
#3787 = CARTESIAN_POINT ( 'NONE',  ( 50.79999999999999716, -3568.700000000000273, 2239.771999999999935 ) ) ;
#3788 = ORIENTED_EDGE ( 'NONE', *, *, #18377, .T. ) ;
#3789 = ADVANCED_FACE ( 'NONE', ( #11377 ), #12633, .T. ) ;
#3790 = AXIS2_PLACEMENT_3D ( 'NONE', #19009, #3062, #8814 ) ;
#3791 = LINE ( 'NONE', #18207, #6996 ) ;
#3792 = DIRECTION ( 'NONE',  ( 0.000000000000000000, 0.000000000000000000, 1.000000000000000000 ) ) ;
#3793 = DIRECTION ( 'NONE',  ( -1.417468298637000021E-14, -1.000000000000000000, -1.484475890936000021E-12 ) ) ;
#3794 = DIRECTION ( 'NONE',  ( 0.000000000000000000, -1.000000000000000000, 0.000000000000000000 ) ) ;
#3795 = DATE_TIME_ROLE ( 'classification_date' ) ;
#3796 = ORIENTED_EDGE ( 'NONE', *, *, #22442, .T. ) ;
#3797 = DIRECTION ( 'NONE',  ( -0.8660254037826616846, 0.5000000000030777603, 0.000000000000000000 ) ) ;
#3798 = ORIENTED_EDGE ( 'NONE', *, *, #16236, .F. ) ;
#3799 = EDGE_CURVE ( 'NONE', #2593, #17406, #717, .T. ) ;
#3800 = ADVANCED_FACE ( 'NONE', ( #11493 ), #2484, .T. ) ;
#3801 = DIRECTION ( 'NONE',  ( 0.000000000000000000, 0.000000000000000000, -1.000000000000000000 ) ) ;
#3802 = VERTEX_POINT ( 'NONE', #20402 ) ;
#3803 = CARTESIAN_POINT ( 'NONE',  ( 8.027948531603557925, -3662.797778259959614, 2246.366055962258542 ) ) ;
#3804 = EDGE_LOOP ( 'NONE', ( #9544, #2399, #15395, #2968 ) ) ;
#3805 = AXIS2_PLACEMENT_3D ( 'NONE', #20772, #4601, #4953 ) ;
#3806 = FACE_OUTER_BOUND ( 'NONE', #5199, .T. ) ;
#3807 = CIRCLE ( 'NONE', #11651, 3.606799999998994366 ) ;
#3808 = CARTESIAN_POINT ( 'NONE',  ( 15.03168679714000078, -3600.843699999999899, 2292.781800000000203 ) ) ;
#3809 = DIRECTION ( 'NONE',  ( -1.000000000000000000, 0.000000000000000000, 0.000000000000000000 ) ) ;
#3810 = CARTESIAN_POINT ( 'NONE',  ( 12.69999999999999929, -3661.409999999999400, 2272.030000000000200 ) ) ;
#3811 = CARTESIAN_POINT ( 'NONE',  ( 18.14025602003983906, -3657.753732795579708, 2245.841877976950400 ) ) ;
#3812 = VERTEX_POINT ( 'NONE', #9292 ) ;
#3813 = DIRECTION ( 'NONE',  ( -1.000000000000000000, 0.000000000000000000, 0.000000000000000000 ) ) ;
#3814 = EDGE_CURVE ( 'NONE', #3057, #15909, #6382, .T. ) ;
#3815 = DIRECTION ( 'NONE',  ( 0.000000000000000000, 0.000000000000000000, -1.000000000000000000 ) ) ;
#3816 = SHAPE_REPRESENTATION ( 'Roller 1', ( #5611 ), #9349 ) ;
#3817 = AXIS2_PLACEMENT_3D ( 'NONE', #18692, #4296, #20461 ) ;
#3818 = CARTESIAN_POINT ( 'NONE',  ( 15.03168679716000078, -3578.148799999999937, 2242.820000000000164 ) ) ;
#3819 = DIRECTION ( 'NONE',  ( 0.000000000000000000, -1.000000000000000000, 0.000000000000000000 ) ) ;
#3820 = CARTESIAN_POINT ( 'NONE',  ( 142.2399999999999807, -3544.490134411880717, 2255.773999999999432 ) ) ;
#3821 = CARTESIAN_POINT ( 'NONE',  ( 137.0230491797765637, -3695.298184790851792, 2255.430966980177800 ) ) ;
#3822 = AXIS2_PLACEMENT_3D ( 'NONE', #15328, #6086, #9594 ) ;
#3823 = AXIS2_PLACEMENT_3D ( 'NONE', #16376, #12857, #3831 ) ;
#3824 = CARTESIAN_POINT ( 'NONE',  ( -8.890000000017000303, -3577.513800000000174, 2249.723686796999573 ) ) ;
#3825 = ORIENTED_EDGE ( 'NONE', *, *, #8014, .F. ) ;
#3826 = PERSON_AND_ORGANIZATION ( #5446, #1895 ) ;
#3827 = AXIS2_PLACEMENT_3D ( 'NONE', #16734, #13103, #9806 ) ;
#3828 = DIRECTION ( 'NONE',  ( 1.000000000000000000, 0.000000000000000000, 0.000000000000000000 ) ) ;
#3829 = DIRECTION ( 'NONE',  ( -0.8660254037840939834, -0.5000000000005969669, 0.000000000000000000 ) ) ;
#3830 = APPROVAL_STATUS ( 'not_yet_approved' ) ;
#3831 = DIRECTION ( 'NONE',  ( 0.000000000000000000, 0.000000000000000000, 1.000000000000000000 ) ) ;
#3832 = FACE_OUTER_BOUND ( 'NONE', #22772, .T. ) ;
#3833 = AXIS2_PLACEMENT_3D ( 'NONE', #14709, #5811, #5462 ) ;
#3834 = DIRECTION ( 'NONE',  ( -4.553079989440860501E-14, 1.000000000000000000, 0.000000000000000000 ) ) ;
#3835 = EDGE_CURVE ( 'NONE', #2645, #17044, #3637, .T. ) ;
#3836 = ADVANCED_FACE ( 'NONE', ( #15022 ), #16425, .T. ) ;
#3837 = ADVANCED_FACE ( 'NONE', ( #13250 ), #9274, .T. ) ;
#3838 = ORIENTED_EDGE ( 'NONE', *, *, #18375, .F. ) ;
#3839 = DIRECTION ( 'NONE',  ( 1.000000000000000000, 0.000000000000000000, 0.000000000000000000 ) ) ;
#3840 = VERTEX_POINT ( 'NONE', #9404 ) ;
#3841 = AXIS2_PLACEMENT_3D ( 'NONE', #22084, #7807, #2744 ) ;
#3842 = LINE ( 'NONE', #16383, #18171 ) ;
#3843 = AXIS2_PLACEMENT_3D ( 'NONE', #756, #19013, #6056 ) ;
#3844 = CARTESIAN_POINT ( 'NONE',  ( 11.47173590547000011, -3636.929856508999819, 2279.750831905999803 ) ) ;
#3845 = VERTEX_POINT ( 'NONE', #2588 ) ;
#3846 = EDGE_CURVE ( 'NONE', #1882, #923, #17866, .T. ) ;
#3847 = DIRECTION ( 'NONE',  ( -1.000000000000000000, 0.000000000000000000, 0.000000000000000000 ) ) ;
#3848 = CIRCLE ( 'NONE', #19952, 2.844800000000091700 ) ;
#3849 = VERTEX_POINT ( 'NONE', #4012 ) ;
#3850 = CARTESIAN_POINT ( 'NONE',  ( 142.7013569010373146, -3695.699999999983902, 2254.618513953578713 ) ) ;
#3851 = DIRECTION ( 'NONE',  ( -1.000000000000000000, 0.000000000000000000, 0.000000000000000000 ) ) ;
#3852 = AXIS2_PLACEMENT_3D ( 'NONE', #3401, #14423, #1639 ) ;
#3853 = EDGE_CURVE ( 'NONE', #11610, #17406, #21930, .T. ) ;
#3854 = ORIENTED_EDGE ( 'NONE', *, *, #1578, .F. ) ;
#3855 = EDGE_CURVE ( 'NONE', #3639, #2356, #6278, .T. ) ;
#3856 = CARTESIAN_POINT ( 'NONE',  ( 137.8408795312830932, -3581.648507417375640, 2247.961733200111667 ) ) ;
#3857 = VERTEX_POINT ( 'NONE', #7633 ) ;
#3859 = DIRECTION ( 'NONE',  ( -0.000000000000000000, -1.000000000000000000, -0.000000000000000000 ) ) ;
#3858 = AXIS2_PLACEMENT_3D ( 'NONE', #13500, #20528, #6143 ) ;
#3860 = DATE_AND_TIME ( #16507, #7139 ) ;
#3861 = CIRCLE ( 'NONE', #2380, 2.844800000000001550 ) ;
#3862 = CARTESIAN_POINT ( 'NONE',  ( 76.20000000000000284, -3670.300000000000182, 2261.869999999999891 ) ) ;
#3863 = CARTESIAN_POINT ( 'NONE',  ( 9.855199999999999960, -3599.497499999999945, 2263.571799999999712 ) ) ;
#3864 = CARTESIAN_POINT ( 'NONE',  ( 10.36831320285999958, -3658.158799999999701, 2242.820000000000164 ) ) ;
#3865 = EDGE_CURVE ( 'NONE', #3889, #15577, #4425, .T. ) ;
#3866 = CARTESIAN_POINT ( 'NONE',  ( 104.4447999999999865, -3619.500000000000000, 2259.837999999999738 ) ) ;
#3867 = ORIENTED_EDGE ( 'NONE', *, *, #7657, .T. ) ;
#3868 = AXIS2_PLACEMENT_3D ( 'NONE', #18970, #9820, #13697 ) ;
#3869 = CARTESIAN_POINT ( 'NONE',  ( 134.6728313949629126, -3576.776753335464946, 2245.454731746178368 ) ) ;
#3871 = ORIENTED_EDGE ( 'NONE', *, *, #2237, .T. ) ;
#3870 = VECTOR ( 'NONE', #3593, 1000.000000000000000 ) ;
#3872 = CARTESIAN_POINT ( 'NONE',  ( 2.859369265473000077, -3695.699999999999818, 2275.763800000000174 ) ) ;
#3873 = EDGE_LOOP ( 'NONE', ( #21688, #3433, #17455, #3027, #19839, #15558 ) ) ;
#3874 = CYLINDRICAL_SURFACE ( 'NONE', #17366, 0.7619999999999294005 ) ;
#3875 = DIRECTION ( 'NONE',  ( 1.000000000000000000, 0.000000000000000000, 0.000000000000000000 ) ) ;
#3876 = AXIS2_PLACEMENT_3D ( 'NONE', #21562, #3974, #18264 ) ;
#3877 = AXIS2_PLACEMENT_3D ( 'NONE', #21459, #16411, #5766 ) ;
#3878 = ORIENTED_EDGE ( 'NONE', *, *, #13239, .F. ) ;
#3879 = FACE_OUTER_BOUND ( 'NONE', #21281, .T. ) ;
#3880 = DIRECTION ( 'NONE',  ( 0.000000000000000000, -1.000000000000000000, 0.000000000000000000 ) ) ;
#3881 = ORIENTED_EDGE ( 'NONE', *, *, #16999, .F. ) ;
#3882 = FACE_OUTER_BOUND ( 'NONE', #20720, .T. ) ;
#3883 = CARTESIAN_POINT ( 'NONE',  ( 10.00591156675000093, -3640.434449278999637, 2279.486295382999742 ) ) ;
#3884 = CARTESIAN_POINT ( 'NONE',  ( 141.6126318482000102, -3581.600863517000107, 2246.630000000000109 ) ) ;
#3885 = ORIENTED_EDGE ( 'NONE', *, *, #3295, .F. ) ;
#3886 = CARTESIAN_POINT ( 'NONE',  ( 12.69999999999999929, -3637.597499999999854, 2264.841800000000148 ) ) ;
#3887 = TOROIDAL_SURFACE ( 'NONE', #874, 4.114799999999999791, 1.270000000000000018 ) ;
#3888 = PERSON_AND_ORGANIZATION_ROLE ( 'classification_officer' ) ;
#3889 = VERTEX_POINT ( 'NONE', #14792 ) ;
#3890 = CARTESIAN_POINT ( 'NONE',  ( 0.000000000000000000, -3544.061999999999898, 2282.113800000000083 ) ) ;
#3891 = CARTESIAN_POINT ( 'NONE',  ( 5.080000000000000071, -3694.430000000000291, 2260.600000000000364 ) ) ;
#3892 = VERTEX_POINT ( 'NONE', #2369 ) ;
#3893 = CARTESIAN_POINT ( 'NONE',  ( 18.12625886363281680, -3581.288617098281520, 2245.910525600300844 ) ) ;
#3894 = CARTESIAN_POINT ( 'NONE',  ( 137.6837585684422436, -3657.497605245348495, 2248.447085333438281 ) ) ;
#3895 = EDGE_LOOP ( 'NONE', ( #11821, #11206, #16120 ) ) ;
#3896 = ORIENTED_EDGE ( 'NONE', *, *, #1346, .F. ) ;
#3897 = CARTESIAN_POINT ( 'NONE',  ( 140.4495444393403716, -3662.249331053435071, 2249.300837621843584 ) ) ;
#3898 = PRODUCT_RELATED_PRODUCT_CATEGORY ( 'detail', '', ( #15546 ) ) ;
#3899 = ORIENTED_EDGE ( 'NONE', *, *, #23035, .F. ) ;
#3900 = VERTEX_POINT ( 'NONE', #6004 ) ;
#3901 = EDGE_LOOP ( 'NONE', ( #9269, #18319, #22768, #18792 ) ) ;
#3902 = TOROIDAL_SURFACE ( 'NONE', #2400, 5.080000000000000071, 0.3810000000000000053 ) ;
#3903 = CARTESIAN_POINT ( 'NONE',  ( 9.880094305751999428, -3579.102405584999815, 2250.228735751999920 ) ) ;
#3904 = EDGE_CURVE ( 'NONE', #5428, #20995, #16739, .T. ) ;
#3905 = AXIS2_PLACEMENT_3D ( 'NONE', #18230, #535, #2188 ) ;
#3906 = EDGE_LOOP ( 'NONE', ( #2371, #12479, #8784, #20494 ) ) ;
#3907 = ORIENTED_EDGE ( 'NONE', *, *, #12800, .F. ) ;
#3908 = DIRECTION ( 'NONE',  ( -0.8660254037817868289, -0.5000000000045929927, 1.319534125262979913E-12 ) ) ;
#3909 = CARTESIAN_POINT ( 'NONE',  ( -12.31900000000000084, -3658.793799999878502, 2245.060313203211081 ) ) ;
#3910 = ADVANCED_FACE ( 'NONE', ( #1288 ), #20869, .T. ) ;
#3911 = ORIENTED_EDGE ( 'NONE', *, *, #10259, .T. ) ;
#3912 = LINE ( 'NONE', #2042, #17444 ) ;
#3913 =( NAMED_UNIT ( * ) SI_UNIT ( $, .STERADIAN. ) SOLID_ANGLE_UNIT ( ) );
#3914 = DIRECTION ( 'NONE',  ( 0.000000000000000000, -1.000000000000000000, 0.000000000000000000 ) ) ;
#3915 = FACE_OUTER_BOUND ( 'NONE', #13642, .T. ) ;
#3916 = DATE_AND_TIME ( #19750, #3398 ) ;
#3917 = CARTESIAN_POINT ( 'NONE',  ( -12.69999999986624495, -3658.702685254810149, 2249.881502164143058 ) ) ;
#3918 = VERTEX_POINT ( 'NONE', #2700 ) ;
#3919 = AXIS2_PLACEMENT_3D ( 'NONE', #13904, #14144, #3460 ) ;
#3920 = CARTESIAN_POINT ( 'NONE',  ( 1.270000000000000018, -3578.860000000000127, 2247.392000000000280 ) ) ;
#3921 = CARTESIAN_POINT ( 'NONE',  ( 8.088613972621001125, -3662.880847139000252, 2246.630000000000109 ) ) ;
#3922 = CIRCLE ( 'NONE', #22623, 0.7619999999999294005 ) ;
#3923 = DIRECTION ( 'NONE',  ( 0.000000000000000000, -1.000000000000000000, 0.000000000000000000 ) ) ;
#3924 = ORIENTED_EDGE ( 'NONE', *, *, #1965, .T. ) ;
#3925 = CARTESIAN_POINT ( 'NONE',  ( 25.39999999999999858, -3568.700000000000273, 2259.837999999999738 ) ) ;
#3926 = CARTESIAN_POINT ( 'NONE',  ( 10.36831320286038327, -3578.148799999852145, 2239.167815367324692 ) ) ;
#3927 = DIRECTION ( 'NONE',  ( 0.000000000000000000, 0.000000000000000000, -1.000000000000000000 ) ) ;
#3928 = DIRECTION ( 'NONE',  ( -1.000000000000000000, 0.000000000000000000, 0.000000000000000000 ) ) ;
#3929 = CARTESIAN_POINT ( 'NONE',  ( 18.06698106831952089, -3657.540322655302134, 2246.234995830579010 ) ) ;
#3930 = EDGE_CURVE ( 'NONE', #3416, #6172, #11956, .T. ) ;
#3931 = ORIENTED_EDGE ( 'NONE', *, *, #705, .T. ) ;
#3932 = DIRECTION ( 'NONE',  ( -0.8660254037817188832, 0.5000000000047110094, 0.000000000000000000 ) ) ;
#3933 = AXIS2_PLACEMENT_3D ( 'NONE', #19711, #17934, #17827 ) ;
#3934 = DIRECTION ( 'NONE',  ( 0.000000000000000000, 0.000000000000000000, 1.000000000000000000 ) ) ;
#3935 = EDGE_CURVE ( 'NONE', #2255, #11877, #11139, .T. ) ;
#3936 = DIRECTION ( 'NONE',  ( 0.000000000000000000, 0.000000000000000000, -1.000000000000000000 ) ) ;
#3938 = EDGE_CURVE ( 'NONE', #22780, #23086, #16172, .T. ) ;
#3937 = AXIS2_PLACEMENT_3D ( 'NONE', #6911, #14181, #5033 ) ;
#3939 = DIRECTION ( 'NONE',  ( 0.000000000000000000, 0.000000000000000000, -1.000000000000000000 ) ) ;
#3940 = CIRCLE ( 'NONE', #579, 2.844799999999994444 ) ;
#3941 = CARTESIAN_POINT ( 'NONE',  ( 142.2559700947606416, -3544.251379751714467, 2255.734053407719330 ) ) ;
#3942 = CARTESIAN_POINT ( 'NONE',  ( 142.0316867971999955, -3658.158799999999701, 2242.820000000000164 ) ) ;
#3943 = CARTESIAN_POINT ( 'NONE',  ( 7.365006562230047571, -3577.445405246308383, 2244.922385902951191 ) ) ;
#3944 = ORIENTED_EDGE ( 'NONE', *, *, #8005, .T. ) ;
#3945 = COORDINATED_UNIVERSAL_TIME_OFFSET ( 0, 0, .AHEAD. ) ;
#3946 = EDGE_LOOP ( 'NONE', ( #15587, #17728 ) ) ;
#3947 = DIRECTION ( 'NONE',  ( -1.000000000000000000, 0.000000000000000000, 0.000000000000000000 ) ) ;
#3948 = CARTESIAN_POINT ( 'NONE',  ( 17.78000000000000114, -3659.504999999999654, 2239.009999999999764 ) ) ;
#3949 = PERSON_AND_ORGANIZATION ( #13271, #22108 ) ;
#3950 = CARTESIAN_POINT ( 'NONE',  ( 0.000000000000000000, -3544.570000000000164, 2259.329999999999927 ) ) ;
#3951 = DIRECTION ( 'NONE',  ( 1.000000000000000000, 0.000000000000000000, 0.000000000000000000 ) ) ;
#3952 = EDGE_CURVE ( 'NONE', #6059, #18860, #10007, .T. ) ;
#3953 = AXIS2_PLACEMENT_3D ( 'NONE', #18002, #10855, #2299 ) ;
#3954 = AXIS2_PLACEMENT_3D ( 'NONE', #10766, #17909, #1859 ) ;
#3955 = CARTESIAN_POINT ( 'NONE',  ( 134.8602052428276181, -3662.544438751693178, 2245.871466275956209 ) ) ;
#3956 = AXIS2_PLACEMENT_3D ( 'NONE', #8400, #1120, #8279 ) ;
#3957 = CARTESIAN_POINT ( 'NONE',  ( 61.26424768829000556, -3543.299999999999727, 2279.065800000000309 ) ) ;
#3958 = VERTEX_POINT ( 'NONE', #21102 ) ;
#3959 =( BOUNDED_CURVE ( )  B_SPLINE_CURVE ( 3, ( #16933, #11777, #13543, #8392 ),
 .UNSPECIFIED., .F., .T. ) 
 B_SPLINE_CURVE_WITH_KNOTS ( ( 4, 4 ),
 ( 1.570796326732663450, 3.141592653589793116 ),
 .UNSPECIFIED. ) 
 CURVE ( )  GEOMETRIC_REPRESENTATION_ITEM ( )  RATIONAL_B_SPLINE_CURVE ( ( 1.000000000000000000, 0.8047378541096965598, 0.8047378541096965598, 1.000000000000000000 ) ) 
 REPRESENTATION_ITEM ( '' )  );
#3960 = CARTESIAN_POINT ( 'NONE',  ( 12.69999999999999929, -3599.497499999999945, 2288.971800000000258 ) ) ;
#3961 = DIRECTION ( 'NONE',  ( 0.000000000000000000, -1.000000000000000000, 0.000000000000000000 ) ) ;
#3962 = ORIENTED_EDGE ( 'NONE', *, *, #182, .F. ) ;
#3963 = CARTESIAN_POINT ( 'NONE',  ( 7.387125747152000876, -3657.399152860999493, 2246.630000000000109 ) ) ;
#3964 = EDGE_CURVE ( 'NONE', #17959, #8199, #2168, .T. ) ;
#3965 = ORIENTED_EDGE ( 'NONE', *, *, #12435, .F. ) ;
#3966 = CARTESIAN_POINT ( 'NONE',  ( 142.2559348849416381, -3694.748620251596094, 2255.734039348222268 ) ) ;
#3967 = DIRECTION ( 'NONE',  ( 1.000000000000000000, 0.000000000000000000, 0.000000000000000000 ) ) ;
#3968 = CIRCLE ( 'NONE', #8475, 0.7620000000000000107 ) ;
#3969 = CIRCLE ( 'NONE', #17420, 2.844799999998995244 ) ;
#3970 = ORIENTED_EDGE ( 'NONE', *, *, #15959, .F. ) ;
#3971 = EDGE_CURVE ( 'NONE', #17006, #12726, #8899, .T. ) ;
#3972 = CIRCLE ( 'NONE', #13318, 0.7620000000000001217 ) ;
#3973 = EDGE_CURVE ( 'NONE', #21577, #3605, #2520, .T. ) ;
#3974 = DIRECTION ( 'NONE',  ( 0.000000000000000000, 1.000000000000000000, 0.000000000000000000 ) ) ;
#3975 = ORIENTED_EDGE ( 'NONE', *, *, #17116, .F. ) ;
#3976 = DIRECTION ( 'NONE',  ( 0.000000000000000000, 0.000000000000000000, 1.000000000000000000 ) ) ;
#3977 = DATE_AND_TIME ( #18495, #8623 ) ;
#3978 = VECTOR ( 'NONE', #2931, 1000.000000000000000 ) ;
#3979 = CARTESIAN_POINT ( 'NONE',  ( 12.80540748638049386, -3642.347302934894742, 2279.817638395105860 ) ) ;
#3980 = DIRECTION ( 'NONE',  ( -1.000000000000000000, 0.000000000000000000, 0.000000000000000000 ) ) ;
#3981 = EDGE_CURVE ( 'NONE', #10237, #21628, #22378, .T. ) ;
#3982 = B_SPLINE_CURVE_WITH_KNOTS ( 'NONE', 3,
 ( #3661, #19729, #21712, #19606, #15972, #2149, #19487, #7186, #7420, #5557, #10810, #18075, #5663, #12802, #19957, #9054, #3894, #10698, #7076, #12689, #14456, #21254, #11042, #155, #18191, #3772, #9296, #19837, #10926, #5313, #2026, #22987, #6960, #14105, #5198, #10583, #17847, #37, #21484, #12457, #17720, #1668, #5430, #8827, #23106, #16088, #14219, #14340, #3540, #13039, #7527, #719, #16773 ),
 .UNSPECIFIED., .F., .F.,
 ( 4, 2, 2, 2, 2, 1, 2, 2, 2, 2, 1, 1, 1, 2, 2, 2, 2, 2, 2, 1, 1, 2, 2, 2, 2, 1, 2, 2, 2, 4 ),
 ( 0.000000000000000000, 0.1249999999841666931, 0.1874999999764063452, 0.2499999999686460250, 0.3124999999608856771, 0.3437499999571574927, 0.3593749999553250141, 0.3749999999534924799, 0.4374999999467432121, 0.4687499999434819875, 0.4843749999417981122, 0.4921874999409536211, 0.4960937499405312923, 0.4980468749403176298, 0.4999999999401039119, 0.5312499999398715422, 0.5624999999396390615, 0.5937499999394066919, 0.6093749999393713868, 0.6171874999394474370, 0.6210937499395690065, 0.6230468749397405359, 0.6249999999399119543, 0.6874999999489770364, 0.7187499999536707262, 0.7343749999559984198, 0.7421874999571623777, 0.7499999999583262245, 0.8749999999791631122, 1.000000000000000000 ),
 .UNSPECIFIED. ) ;
#3983 = DIRECTION ( 'NONE',  ( -1.000000000000000000, 0.000000000000000000, 0.000000000000000000 ) ) ;
#3984 = CARTESIAN_POINT ( 'NONE',  ( 114.2999999999999972, -3594.099999999999909, 2259.837999999999738 ) ) ;
#3985 = CARTESIAN_POINT ( 'NONE',  ( 140.5955809558492149, -3576.794761112849756, 2249.348465679632682 ) ) ;
#3986 = ORIENTED_EDGE ( 'NONE', *, *, #21004, .F. ) ;
#3987 = CARTESIAN_POINT ( 'NONE',  ( 134.4913178369996842, -3577.143244214250444, 2245.123591688256056 ) ) ;
#3988 = EDGE_CURVE ( 'NONE', #21259, #20612, #15361, .T. ) ;
#3989 = CIRCLE ( 'NONE', #2860, 0.3809999999999647002 ) ;
#3990 = EDGE_CURVE ( 'NONE', #19181, #7611, #5048, .T. ) ;
#3991 = VERTEX_POINT ( 'NONE', #17335 ) ;
#3992 = DIRECTION ( 'NONE',  ( 0.000000000000000000, -2.336881798971000105E-14, 1.000000000000000000 ) ) ;
#3993 = EDGE_LOOP ( 'NONE', ( #3965, #18312, #10822, #19610 ) ) ;
#3994 = CARTESIAN_POINT ( 'NONE',  ( 12.60780787143999859, -3582.339800030000333, 2257.592639999999847 ) ) ;
#3995 = VECTOR ( 'NONE', #582, 1000.000000000000000 ) ;
#3996 = FACE_OUTER_BOUND ( 'NONE', #1343, .T. ) ;
#3997 = CIRCLE ( 'NONE', #7001, 3.606800000000000228 ) ;
#3998 = ORIENTED_EDGE ( 'NONE', *, *, #3083, .T. ) ;
#3999 = CARTESIAN_POINT ( 'NONE',  ( -8.890000000024000926, -3657.447599999999966, 2247.392000000000280 ) ) ;
#4000 = DIRECTION ( 'NONE',  ( 0.000000000000000000, 1.000000000000000000, 0.000000000000000000 ) ) ;
#4001 = ORIENTED_EDGE ( 'NONE', *, *, #16023, .T. ) ;
#4002 = DIRECTION ( 'NONE',  ( 3.433625482341074198E-14, 0.5000000000047110094, 0.8660254037817188832 ) ) ;
#4003 = EDGE_CURVE ( 'NONE', #8533, #3605, #5534, .T. ) ;
#4004 = CARTESIAN_POINT ( 'NONE',  ( 10.71531464684066393, -3577.456266983200749, 2249.866613545771088 ) ) ;
#4005 = DIRECTION ( 'NONE',  ( 0.000000000000000000, 0.000000000000000000, 1.000000000000000000 ) ) ;
#4006 = FACE_OUTER_BOUND ( 'NONE', #21444, .T. ) ;
#4007 = EDGE_LOOP ( 'NONE', ( #9677, #16560, #13283, #14138 ) ) ;
#4008 = CIRCLE ( 'NONE', #22742, 2.844800000000091700 ) ;
#4009 = DIRECTION ( 'NONE',  ( 0.000000000000000000, 0.000000000000000000, -1.000000000000000000 ) ) ;
#4010 = SHAPE_DEFINITION_REPRESENTATION ( #15743, #1421 ) ;
#4011 = AXIS2_PLACEMENT_3D ( 'NONE', #10454, #19017, #23096 ) ;
#4012 = CARTESIAN_POINT ( 'NONE',  ( -0.7620000000000000107, -3578.860000000000127, 2244.547199999999975 ) ) ;
#4013 = CARTESIAN_POINT ( 'NONE',  ( -12.31900000000002748, -3580.206200000138779, 2245.060313203175610 ) ) ;
#4014 = EDGE_LOOP ( 'NONE', ( #2973, #10326, #10370, #21609 ) ) ;
#4015 = DIRECTION ( 'NONE',  ( 0.000000000000000000, 0.000000000000000000, -1.000000000000000000 ) ) ;
#4016 = CARTESIAN_POINT ( 'NONE',  ( 137.8194210030732449, -3577.352480115512208, 2257.752117387002727 ) ) ;
#4017 = VERTEX_POINT ( 'NONE', #18751 ) ;
#4018 = AXIS2_PLACEMENT_3D ( 'NONE', #18520, #20616, #930 ) ;
#4019 = ORIENTED_EDGE ( 'NONE', *, *, #4790, .F. ) ;
#4020 = CARTESIAN_POINT ( 'NONE',  ( 137.3526213507248315, -3661.114307651350828, 2250.065742440782742 ) ) ;
#4021 = ADVANCED_FACE ( 'NONE', ( #13605 ), #22731, .T. ) ;
#4022 = VERTEX_POINT ( 'NONE', #20984 ) ;
#4023 = ORIENTED_EDGE ( 'NONE', *, *, #10946, .F. ) ;
#4024 = AXIS2_PLACEMENT_3D ( 'NONE', #19454, #18992, #22953 ) ;
#4025 = DIRECTION ( 'NONE',  ( 0.000000000000000000, -1.000000000000000000, 0.000000000000000000 ) ) ;
#4026 = ORIENTED_EDGE ( 'NONE', *, *, #8090, .F. ) ;
#4027 = DIRECTION ( 'NONE',  ( 1.000000000000000000, 0.000000000000000000, 0.000000000000000000 ) ) ;
#4028 = CALENDAR_DATE ( 2026, 26, 10 ) ;
#4029 = DIRECTION ( 'NONE',  ( 0.000000000000000000, 0.000000000000000000, -1.000000000000000000 ) ) ;
#4030 = ORIENTED_EDGE ( 'NONE', *, *, #7433, .T. ) ;
#4031 = VECTOR ( 'NONE', #3603, 1000.000000000000000 ) ;
#4032 = CARTESIAN_POINT ( 'NONE',  ( 38.10000000000000142, -3594.099999999999909, 2259.837999999999738 ) ) ;
#4033 = AXIS2_PLACEMENT_3D ( 'NONE', #5781, #18299, #14678 ) ;
#4034 = DIRECTION ( 'NONE',  ( 0.000000000000000000, -1.000000000000000000, 0.000000000000000000 ) ) ;
#4035 = LINE ( 'NONE', #20094, #21831 ) ;
#4036 = DIRECTION ( 'NONE',  ( -1.000000000000000000, 0.000000000000000000, 0.000000000000000000 ) ) ;
#4037 = APPLICATION_PROTOCOL_DEFINITION ( 'international standard', 'automotive_design', 2000, #6476 ) ;
#4038 = CARTESIAN_POINT ( 'NONE',  ( 114.2999999999999972, -3594.099999999999909, 2239.771999999999935 ) ) ;
#4039 = ORIENTED_EDGE ( 'NONE', *, *, #11851, .T. ) ;
#4040 = DIRECTION ( 'NONE',  ( 0.000000000000000000, -1.000000000000000000, 0.000000000000000000 ) ) ;
#4041 = AXIS2_PLACEMENT_3D ( 'NONE', #11345, #9596, #9480 ) ;
#4042 = CARTESIAN_POINT ( 'NONE',  ( 7.719554562072720394, -3662.307856581991018, 2245.543048782076312 ) ) ;
#4043 = ORIENTED_EDGE ( 'NONE', *, *, #13116, .T. ) ;
#4044 = FACE_OUTER_BOUND ( 'NONE', #21478, .T. ) ;
#4045 = AXIS2_PLACEMENT_3D ( 'NONE', #19867, #19986, #5927 ) ;
#4046 = CARTESIAN_POINT ( 'NONE',  ( 142.0316867971266390, -3660.851200000091012, 2239.391000000000076 ) ) ;
#4047 = DIRECTION ( 'NONE',  ( 1.000000000000000000, 0.000000000000000000, 0.000000000000000000 ) ) ;
#4048 = CARTESIAN_POINT ( 'NONE',  ( 16.19063073443439293, -3695.699999999999818, 2282.113800000095125 ) ) ;
#4049 = CARTESIAN_POINT ( 'NONE',  ( 18.20822205038428621, -3657.980541937662565, 2245.538019395683932 ) ) ;
#4050 = VERTEX_POINT ( 'NONE', #8214 ) ;
#4051 = CARTESIAN_POINT ( 'NONE',  ( 147.4346999979424595, -3695.234698870522152, 2260.312749946543590 ) ) ;
#4052 = CARTESIAN_POINT ( 'NONE',  ( 139.6999999999999886, -3662.197400000000016, 2242.820000000000164 ) ) ;
#4053 = DIRECTION ( 'NONE',  ( 0.000000000000000000, 0.000000000000000000, 1.000000000000000000 ) ) ;
#4054 = DIRECTION ( 'NONE',  ( 1.000000000000000000, 0.000000000000000000, 0.000000000000000000 ) ) ;
#4055 = CARTESIAN_POINT ( 'NONE',  ( 142.3295600303597723, -3543.848287275569874, 2255.549808268773177 ) ) ;
#4056 = DIRECTION ( 'NONE',  ( 0.000000000000000000, 0.000000000000000000, -1.000000000000000000 ) ) ;
#4057 = CARTESIAN_POINT ( 'NONE',  ( 7.608775882559566384, -3576.898905879581889, 2245.331008237134029 ) ) ;
#4058 = ORIENTED_EDGE ( 'NONE', *, *, #15539, .T. ) ;
#4059 = APPROVAL_DATE_TIME ( #18804, #21262 ) ;
#4060 = APPROVAL ( #5456, 'UNSPECIFIED' ) ;
#4061 = ORIENTED_EDGE ( 'NONE', *, *, #2237, .F. ) ;
#4062 = DIRECTION ( 'NONE',  ( -1.224646799147353207E-16, 1.000000000000000000, 0.000000000000000000 ) ) ;
#4063 = CARTESIAN_POINT ( 'NONE',  ( 129.8447999999989975, -3568.700000000000273, 2261.869999999999891 ) ) ;
#4064 = CARTESIAN_POINT ( 'NONE',  ( 12.69999999999999929, -3657.599999999999909, 2272.030000000000200 ) ) ;
#4065 = EDGE_CURVE ( 'NONE', #1150, #3958, #10315, .T. ) ;
#4066 = CARTESIAN_POINT ( 'NONE',  ( -8.890000000026999416, -3657.447599999999966, 2247.392000000000280 ) ) ;
#4067 = EDGE_CURVE ( 'NONE', #15488, #11524, #17485, .T. ) ;
#4068 = ORIENTED_EDGE ( 'NONE', *, *, #7235, .T. ) ;
#4069 = CARTESIAN_POINT ( 'NONE',  ( 135.0283457588961653, -3662.798513796493353, 2246.367958887603891 ) ) ;
#4070 = EDGE_CURVE ( 'NONE', #2928, #15033, #4692, .T. ) ;
#4071 = ORIENTED_EDGE ( 'NONE', *, *, #14140, .F. ) ;
#4072 = FACE_OUTER_BOUND ( 'NONE', #17930, .T. ) ;
#4073 = ORIENTED_EDGE ( 'NONE', *, *, #22008, .F. ) ;
#4074 = CIRCLE ( 'NONE', #16792, 5.460999999999938126 ) ;
#4075 = DIRECTION ( 'NONE',  ( 0.000000000000000000, 0.000000000000000000, -1.000000000000000000 ) ) ;
#4076 = APPLICATION_CONTEXT ( 'configuration controlled 3d designs of mechanical parts and assemblies' ) ;
#4077 = CARTESIAN_POINT ( 'NONE',  ( 35.56000000000000227, -3694.430000000000291, 2247.392000000000280 ) ) ;
#4078 = ORIENTED_EDGE ( 'NONE', *, *, #13162, .T. ) ;
#4079 = EDGE_CURVE ( 'NONE', #3526, #13971, #17459, .T. ) ;
#4080 = DIRECTION ( 'NONE',  ( 0.5000000000005969669, -0.8660254037840939834, 0.000000000000000000 ) ) ;
#4081 = CARTESIAN_POINT ( 'NONE',  ( 63.50000000000000000, -3644.899999999999636, 2259.837999999999738 ) ) ;
#4082 = ORIENTED_EDGE ( 'NONE', *, *, #13147, .T. ) ;
#4083 = CARTESIAN_POINT ( 'NONE',  ( 38.10000000000000142, -3644.899999999999636, 2259.837999999999738 ) ) ;
#4084 = LINE ( 'NONE', #18708, #21796 ) ;
#4085 = EDGE_CURVE ( 'NONE', #13188, #13105, #6668, .T. ) ;
#4086 = ORIENTED_EDGE ( 'NONE', *, *, #7098, .F. ) ;
#4087 = DIRECTION ( 'NONE',  ( 2.324635735433000053E-14, 0.000000000000000000, 1.000000000000000000 ) ) ;
#4088 = UNCERTAINTY_MEASURE_WITH_UNIT (LENGTH_MEASURE( 1.000000000000000082E-05 ), #16644, 'distance_accuracy_value', 'NONE');
#4089 = ORIENTED_EDGE ( 'NONE', *, *, #13868, .T. ) ;
#4090 = CIRCLE ( 'NONE', #22045, 3.606800000000021100 ) ;
#4091 = CARTESIAN_POINT ( 'NONE',  ( 145.2535822323377204, -3580.844011437738573, 2245.352786166252372 ) ) ;
#4092 = DATE_AND_TIME ( #5977, #10114 ) ;
#4093 = CARTESIAN_POINT ( 'NONE',  ( 145.4120474421716835, -3579.283774594628539, 2244.576911952362025 ) ) ;
#4094 = FACE_OUTER_BOUND ( 'NONE', #2155, .T. ) ;
#4095 = CARTESIAN_POINT ( 'NONE',  ( 131.7757523116999891, -3544.570000000000164, 2260.600000000000364 ) ) ;
#4096 = ADVANCED_FACE ( 'NONE', ( #3510 ), #10662, .F. ) ;
#4097 = CARTESIAN_POINT ( 'NONE',  ( 0.7620000000000000107, -3694.938000000000102, 2275.763800000000174 ) ) ;
#4098 = CARTESIAN_POINT ( 'NONE',  ( 142.3952936667693905, -3578.572481595138925, 2250.225737411198679 ) ) ;
#4099 = ORIENTED_EDGE ( 'NONE', *, *, #3935, .F. ) ;
#4100 = CIRCLE ( 'NONE', #17927, 3.606800000000000228 ) ;
#4101 = EDGE_CURVE ( 'NONE', #6730, #22793, #6003, .T. ) ;
#4102 = VERTEX_POINT ( 'NONE', #3738 ) ;
#4103 = CARTESIAN_POINT ( 'NONE',  ( 15.24000000000000021, -3544.570000000000164, 2255.774000000000342 ) ) ;
#4104 = VERTEX_POINT ( 'NONE', #19806 ) ;
#4105 = LOCAL_TIME ( 17, 37, 43.00000000000000000, #4720 ) ;
#4106 = CARTESIAN_POINT ( 'NONE',  ( 64.76999999999999602, -3544.061999999999898, 2289.213099999999940 ) ) ;
#4107 = CARTESIAN_POINT ( 'NONE',  ( 142.5447999999990998, -3659.693701068885275, 2257.962944264954785 ) ) ;
#4108 = APPLICATION_CONTEXT ( 'configuration controlled 3d designs of mechanical parts and assemblies' ) ;
#4109 = EDGE_LOOP ( 'NONE', ( #4560, #5563 ) ) ;
#4110 = CARTESIAN_POINT ( 'NONE',  ( -6.730999999999999872, -3660.140000000000327, 2247.392000000000280 ) ) ;
#4111 = CYLINDRICAL_SURFACE ( 'NONE', #480, 2.844800000000091700 ) ;
#4112 = EDGE_LOOP ( 'NONE', ( #13945, #21532, #14018, #4082, #2884 ) ) ;
#4113 = PLANE ( 'NONE',  #19205 ) ;
#4114 = CARTESIAN_POINT ( 'NONE',  ( 12.05677975596295148, -3576.723661194017041, 2249.270583004743003 ) ) ;
#4115 =( NAMED_UNIT ( * ) PLANE_ANGLE_UNIT ( ) SI_UNIT ( $, .RADIAN. ) );
#4116 = DIRECTION ( 'NONE',  ( 0.000000000000000000, -1.000000000000000000, 0.000000000000000000 ) ) ;
#4117 = ORIENTED_EDGE ( 'NONE', *, *, #13511, .F. ) ;
#4118 = CARTESIAN_POINT ( 'NONE',  ( 137.8183059363161362, -3661.646540044306676, 2257.752309761470315 ) ) ;
#4119 = APPROVAL_STATUS ( 'not_yet_approved' ) ;
#4120 = CARTESIAN_POINT ( 'NONE',  ( 20.37131446257999912, -3694.758336080999925, 2260.557504193999648 ) ) ;
#4121 = LINE ( 'NONE', #4659, #14692 ) ;
#4122 = SECURITY_CLASSIFICATION ( '', '', #7986 ) ;
#4123 = CARTESIAN_POINT ( 'NONE',  ( 20.32000000000000028, -3695.699999999999818, 2289.213099999999940 ) ) ;
#4124 = AXIS2_PLACEMENT_3D ( 'NONE', #20863, #2933, #1051 ) ;
#4125 = CARTESIAN_POINT ( 'NONE',  ( -5.588000000000000078, -3578.860000000000127, 2247.392000000000280 ) ) ;
#4126 = VERTEX_POINT ( 'NONE', #12313 ) ;
#4127 = VERTEX_POINT ( 'NONE', #7049 ) ;
#4128 = CARTESIAN_POINT ( 'NONE',  ( 137.3063811338797962, -3661.044633701663770, 2250.090170880306232 ) ) ;
#4129 = ADVANCED_FACE ( 'NONE', ( #7267 ), #19694, .T. ) ;
#4130 = EDGE_LOOP ( 'NONE', ( #612, #14052, #8881, #4584 ) ) ;
#4131 = EDGE_CURVE ( 'NONE', #10003, #20430, #17528, .T. ) ;
#4132 = ORIENTED_EDGE ( 'NONE', *, *, #15536, .F. ) ;
#4133 = AXIS2_PLACEMENT_3D ( 'NONE', #9348, #16485, #21989 ) ;
#4134 = CARTESIAN_POINT ( 'NONE',  ( 29.00679999999900005, -3619.500000000000000, 2260.600000000000364 ) ) ;
#4135 = ORIENTED_EDGE ( 'NONE', *, *, #21053, .F. ) ;
#4136 = APPLIED_APPROVAL_ASSIGNMENT ( #19805, ( #13118 ) ) ;
#4137 = DIRECTION ( 'NONE',  ( 0.000000000000000000, 0.000000000000000000, -1.000000000000000000 ) ) ;
#4138 = APPROVAL_ROLE ( '' ) ;
#4139 = CARTESIAN_POINT ( 'NONE',  ( -6.730999999999999872, -3660.140000000000327, 2247.392000000000280 ) ) ;
#4140 = EDGE_CURVE ( 'NONE', #287, #16201, #10095, .T. ) ;
#4141 = LOCAL_TIME ( 17, 37, 43.00000000000000000, #321 ) ;
#4142 = ORIENTED_EDGE ( 'NONE', *, *, #13409, .T. ) ;
#4143 = CARTESIAN_POINT ( 'NONE',  ( 7.108545037236568831, -3658.323337185065611, 2245.202519759302504 ) ) ;
#4144 = FACE_BOUND ( 'NONE', #18395, .T. ) ;
#4145 = CARTESIAN_POINT ( 'NONE',  ( 12.70000000005999929, -3576.802599999999984, 2242.820000000000164 ) ) ;
#4146 = CARTESIAN_POINT ( 'NONE',  ( 127.0000000000000000, -3670.300000000000182, 2260.600000000000364 ) ) ;
#4147 = EDGE_CURVE ( 'NONE', #5084, #21589, #14226, .T. ) ;
#4148 = PERSON_AND_ORGANIZATION_ROLE ( 'creator' ) ;
#4149 = EDGE_CURVE ( 'NONE', #12180, #957, #20561, .T. ) ;
#4150 = CARTESIAN_POINT ( 'NONE',  ( 25.39999999999999858, -3578.860000000000127, 2244.547199999999975 ) ) ;
#4151 = CARTESIAN_POINT ( 'NONE',  ( 142.3647906480871654, -3658.508756101628933, 2249.722899581812726 ) ) ;
#4152 = CARTESIAN_POINT ( 'NONE',  ( 7.261600995315486529, -3661.299381583153718, 2244.776454689257207 ) ) ;
#4153 = ORGANIZATION ( 'NAUO-ORG7', 'UNSPECIFIED', 'UNSPECIFIED' ) ;
#4154 = APPLIED_APPROVAL_ASSIGNMENT ( #4630, ( #20249 ) ) ;
#4155 = EDGE_LOOP ( 'NONE', ( #11359, #6341, #10311, #11892, #9276, #21554 ) ) ;
#4156 = CYLINDRICAL_SURFACE ( 'NONE', #9597, 0.7620000000000000107 ) ;
#4157 = CARTESIAN_POINT ( 'NONE',  ( 12.69999999999999929, -3599.497499999999945, 2290.622800000000097 ) ) ;
#4158 = ORIENTED_EDGE ( 'NONE', *, *, #12957, .F. ) ;
#4159 = CARTESIAN_POINT ( 'NONE',  ( 12.69999999999999929, -3604.958499999999731, 2290.622800000000097 ) ) ;
#4160 = PRODUCT_DEFINITION_SHAPE ( 'NONE', 'NONE',  #23178 ) ;
#4161 = TOROIDAL_SURFACE ( 'NONE', #7528, 3.606799999999999784, 0.7620000000000000107 ) ;
#4162 = CARTESIAN_POINT ( 'NONE',  ( 18.34551793137252673, -3658.616110195214333, 2244.989057792325184 ) ) ;
#4163 = VERTEX_POINT ( 'NONE', #22955 ) ;
#4164 = CARTESIAN_POINT ( 'NONE',  ( 147.4837490350197982, -3695.367664692139897, 2260.189857417176881 ) ) ;
#4165 = DIRECTION ( 'NONE',  ( 0.5000000000047859494, 0.8660254037816754735, 0.000000000000000000 ) ) ;
#4166 = DIRECTION ( 'NONE',  ( -0.8660254037842740615, 0.5000000000002851053, 3.628718844334890455E-12 ) ) ;
#4167 = DIRECTION ( 'NONE',  ( -1.000000000000000000, 0.000000000000000000, 0.000000000000000000 ) ) ;
#4168 = CARTESIAN_POINT ( 'NONE',  ( 142.3769508200778375, -3543.701815209601591, 2255.430966980605717 ) ) ;
#4169 = DIRECTION ( 'NONE',  ( -2.848935406719999894E-12, 1.000000000000000000, 0.000000000000000000 ) ) ;
#4170 = APPLIED_APPROVAL_ASSIGNMENT ( #5473, ( #9761 ) ) ;
#4171 = CARTESIAN_POINT ( 'NONE',  ( 7.176225798281845591, -3578.028891693621517, 2244.671246062090177 ) ) ;
#4172 = ORIENTED_EDGE ( 'NONE', *, *, #9441, .F. ) ;
#4173 = PERSON_AND_ORGANIZATION ( #5446, #1895 ) ;
#4174 = VERTEX_POINT ( 'NONE', #14303 ) ;
#4175 = CARTESIAN_POINT ( 'NONE',  ( 145.0670228868914933, -3657.540459061100591, 2246.234687787927669 ) ) ;
#4176 = VECTOR ( 'NONE', #1227, 1000.000000000000000 ) ;
#4177 = AXIS2_PLACEMENT_3D ( 'NONE', #9418, #16557, #7649 ) ;
#4178 = DIRECTION ( 'NONE',  ( 0.000000000000000000, -1.000000000000000000, 0.000000000000000000 ) ) ;
#4179 = CARTESIAN_POINT ( 'NONE',  ( 12.69999999999999929, -3599.497499999999945, 2281.351799999999912 ) ) ;
#4180 = ORIENTED_EDGE ( 'NONE', *, *, #22002, .F. ) ;
#4181 = CARTESIAN_POINT ( 'NONE',  ( 12.69999999999999929, -3639.502500000000055, 2296.210799999999836 ) ) ;
#4182 = ORIENTED_EDGE ( 'NONE', *, *, #9547, .T. ) ;
#4183 = LINE ( 'NONE', #670, #2770 ) ;
#4184 = ORIENTED_EDGE ( 'NONE', *, *, #22869, .T. ) ;
#4185 = CARTESIAN_POINT ( 'NONE',  ( 15.21739391844383960, -3660.839252834448416, 2250.153081304058560 ) ) ;
#4186 = APPROVAL ( #8453, 'UNSPECIFIED' ) ;
#4187 = CARTESIAN_POINT ( 'NONE',  ( 54.40679999999999694, -3670.300000000000182, 2259.837999999999738 ) ) ;
#4188 = ORIENTED_EDGE ( 'NONE', *, *, #4067, .F. ) ;
#4189 = FACE_OUTER_BOUND ( 'NONE', #19073, .T. ) ;
#4190 = AXIS2_PLACEMENT_3D ( 'NONE', #4831, #6490, #2961 ) ;
#4191 = CARTESIAN_POINT ( 'NONE',  ( 116.8400000000000034, -3670.300000000000182, 2250.236800000000130 ) ) ;
#4192 = AXIS2_PLACEMENT_3D ( 'NONE', #10650, #5390, #7516 ) ;
#4193 = ADVANCED_FACE ( 'NONE', ( #12422 ), #21335, .T. ) ;
#4194 = ORIENTED_EDGE ( 'NONE', *, *, #409, .T. ) ;
#4195 = DIRECTION ( 'NONE',  ( -1.000000000000000000, 0.000000000000000000, 0.000000000000000000 ) ) ;
#4196 = CYLINDRICAL_SURFACE ( 'NONE', #5721, 0.3809999999999303388 ) ;
#4197 = EDGE_CURVE ( 'NONE', #16752, #11962, #5621, .T. ) ;
#4198 = ORIENTED_EDGE ( 'NONE', *, *, #17352, .T. ) ;
#4199 = ORIENTED_EDGE ( 'NONE', *, *, #5148, .T. ) ;
#4200 = EDGE_CURVE ( 'NONE', #4775, #22886, #19572, .T. ) ;
#4201 = DIRECTION ( 'NONE',  ( -3.370353031811000117E-12, 1.000000000000000000, 1.649417656554999944E-12 ) ) ;
#4202 = ORIENTED_EDGE ( 'NONE', *, *, #3573, .T. ) ;
#4203 = CARTESIAN_POINT ( 'NONE',  ( 145.2205435179829749, -3580.973142349780119, 2245.487016221928570 ) ) ;
#4205 = AXIS2_PLACEMENT_3D ( 'NONE', #15656, #17751, #16001 ) ;
#4204 = APPROVAL_STATUS ( 'not_yet_approved' ) ;
#4206 = CARTESIAN_POINT ( 'NONE',  ( 15.54479999999999862, -3639.502500000000055, 2279.447335734999797 ) ) ;
#4207 = EDGE_CURVE ( 'NONE', #13662, #12207, #11225, .T. ) ;
#4208 = CARTESIAN_POINT ( 'NONE',  ( 17.73574364357449085, -3662.207325212531487, 2245.437750342633080 ) ) ;
#4209 = AXIS2_PLACEMENT_3D ( 'NONE', #17654, #15792, #1603 ) ;
#4210 = VECTOR ( 'NONE', #17659, 1000.000000000000000 ) ;
#4211 = CARTESIAN_POINT ( 'NONE',  ( -0.7620000000000000107, -3578.860000000000127, 2250.236800000000130 ) ) ;
#4212 = DIRECTION ( 'NONE',  ( -0.8660254037816756956, 0.5000000000047857274, 0.000000000000000000 ) ) ;
#4213 = CIRCLE ( 'NONE', #19927, 1.269999999999882334 ) ;
#4214 = CARTESIAN_POINT ( 'NONE',  ( 140.8264938607258614, -3576.881393884998488, 2249.436472243866319 ) ) ;
#4215 = ORIENTED_EDGE ( 'NONE', *, *, #4834, .T. ) ;
#4216 = CARTESIAN_POINT ( 'NONE',  ( 60.65520000000000067, -3644.899999999999636, 2261.869999999999891 ) ) ;
#4217 = DIRECTION ( 'NONE',  ( 0.000000000000000000, -2.336881798971000105E-14, -1.000000000000000000 ) ) ;
#4218 = ORIENTED_EDGE ( 'NONE', *, *, #8730, .T. ) ;
#4219 = DIRECTION ( 'NONE',  ( 0.000000000000000000, -1.000000000000000000, 0.000000000000000000 ) ) ;
#4220 = CARTESIAN_POINT ( 'NONE',  ( 15.57690423030046745, -3543.373434453245409, 2254.929879518507278 ) ) ;
#4221 = AXIS2_PLACEMENT_3D ( 'NONE', #15392, #22521, #10109 ) ;
#4222 = ORIENTED_EDGE ( 'NONE', *, *, #13000, .T. ) ;
#4223 = EDGE_CURVE ( 'NONE', #13513, #19068, #5616, .T. ) ;
#4224 = ORIENTED_EDGE ( 'NONE', *, *, #827, .T. ) ;
#4225 = FACE_OUTER_BOUND ( 'NONE', #1802, .T. ) ;
#4226 = AXIS2_PLACEMENT_3D ( 'NONE', #13025, #18829, #4772 ) ;
#4227 = EDGE_CURVE ( 'NONE', #22617, #4557, #10894, .T. ) ;
#4228 = ORIENTED_EDGE ( 'NONE', *, *, #1640, .F. ) ;
#4229 = EDGE_CURVE ( 'NONE', #10620, #13850, #7386, .T. ) ;
#4230 = AXIS2_PLACEMENT_3D ( 'NONE', #7624, #19827, #12676 ) ;
#4231 = DIRECTION ( 'NONE',  ( 0.000000000000000000, 0.000000000000000000, -1.000000000000000000 ) ) ;
#4232 = CARTESIAN_POINT ( 'NONE',  ( 11.49846512652514363, -3576.916035655123324, 2249.469127929353363 ) ) ;
#4233 = CARTESIAN_POINT ( 'NONE',  ( 141.9145117060755297, -3581.280835468015539, 2248.886214331544579 ) ) ;
#4234 = ORIENTED_EDGE ( 'NONE', *, *, #4079, .T. ) ;
#4235 = DIRECTION ( 'NONE',  ( 1.000000000000000000, 0.000000000000000000, 0.000000000000000000 ) ) ;
#4236 =( BOUNDED_CURVE ( )  B_SPLINE_CURVE ( 3, ( #3432, #10347, #17494, #1440 ),
 .UNSPECIFIED., .F., .T. ) 
 B_SPLINE_CURVE_WITH_KNOTS ( ( 4, 4 ),
 ( -9.769962616701377556E-15, 1.570796326960964162 ),
 .UNSPECIFIED. ) 
 CURVE ( )  GEOMETRIC_REPRESENTATION_ITEM ( )  RATIONAL_B_SPLINE_CURVE ( ( 1.000000000000000000, 0.8047378540852202500, 0.8047378540852202500, 1.000000000000000000 ) ) 
 REPRESENTATION_ITEM ( '' )  );
#4237 = DATE_AND_TIME ( #7631, #13465 ) ;
#4238 = CARTESIAN_POINT ( 'NONE',  ( 79.80679999999999552, -3568.700000000000273, 2239.771999999999935 ) ) ;
#4239 = DIRECTION ( 'NONE',  ( 0.000000000000000000, 1.000000000000000000, 0.000000000000000000 ) ) ;
#4240 = ORIENTED_EDGE ( 'NONE', *, *, #8538, .F. ) ;
#4241 = DIRECTION ( 'NONE',  ( 0.000000000000000000, 0.000000000000000000, 1.000000000000000000 ) ) ;
#4242 = CIRCLE ( 'NONE', #4993, 7.111999999999785160 ) ;
#4243 = CARTESIAN_POINT ( 'NONE',  ( 138.4364504168152621, -3576.939413531078117, 2257.663356991057299 ) ) ;
#4244 = EDGE_CURVE ( 'NONE', #749, #4022, #6735, .T. ) ;
#4245 = ORIENTED_EDGE ( 'NONE', *, *, #17133, .F. ) ;
#4246 = CIRCLE ( 'NONE', #19587, 1.269999999999882334 ) ;
#4247 = CARTESIAN_POINT ( 'NONE',  ( 142.0581284917780067, -3661.097254891949433, 2250.071354168025209 ) ) ;
#4248 = ORIENTED_EDGE ( 'NONE', *, *, #7834, .T. ) ;
#4249 = VERTEX_POINT ( 'NONE', #16508 ) ;
#4250 = ORIENTED_EDGE ( 'NONE', *, *, #17246, .F. ) ;
#4251 = CARTESIAN_POINT ( 'NONE',  ( 139.6999999999999886, -3579.494999999999891, 2272.030000000000200 ) ) ;
#4252 = EDGE_LOOP ( 'NONE', ( #23082, #10266, #5772, #4132 ) ) ;
#4253 = LINE ( 'NONE', #2499, #13903 ) ;
#4254 = FACE_OUTER_BOUND ( 'NONE', #19590, .T. ) ;
#4255 = TOROIDAL_SURFACE ( 'NONE', #4612, 1.905000000000000027, 1.270000000000000018 ) ;
#4256 = ORIENTED_EDGE ( 'NONE', *, *, #7221, .F. ) ;
#4257 = PLANE ( 'NONE',  #2122 ) ;
#4258 =( NAMED_UNIT ( * ) PLANE_ANGLE_UNIT ( ) SI_UNIT ( $, .RADIAN. ) );
#4259 = DIRECTION ( 'NONE',  ( 0.000000000000000000, -1.000000000000000000, 0.000000000000000000 ) ) ;
#4260 = B_SPLINE_CURVE_WITH_KNOTS ( 'NONE', 3,
 ( #4526, #18479, #13434, #4418, #4185, #18702, #9908, #7823, #15202, #883, #11789, #10034, #13201, #8050, #8170, #6306, #775, #11662, #7708, #20244, #9690, #14972, #18821, #2765, #17057, #11446, #1008, #14864, #20693, #11330, #22440, #6415, #4640, #2435, #4306, #674, #18943, #17176, #9578, #16724, #22104, #20357, #18596, #12029, #14024, #3347, #17289, #10500, #22791, #10616, #14147, #8751, #21057, #22564, #4876, #23028, #17641, #10149, #1591, #22908, #8523, #20936, #1241, #15545, #10384, #12140, #7002, #6885, #5002, #19410, #15897, #13792, #19179, #22683, #6656, #12267, #13907, #3001, #21175, #15430, #5124, #21293, #3115, #5235, #12376, #15780, #1472, #10264, #17524, #19524, #8630, #3464 ),
 .UNSPECIFIED., .F., .F.,
 ( 4, 2, 2, 2, 1, 1, 2, 2, 2, 2, 1, 2, 2, 2, 2, 1, 2, 2, 2, 2, 2, 2, 2, 2, 2, 2, 2, 2, 1, 2, 2, 2, 2, 1, 1, 2, 2, 2, 1, 2, 2, 1, 2, 2, 2, 2, 1, 2, 2, 2, 4 ),
 ( 0.000000000000000000, 0.06250000000004160561, 0.1250000000000832112, 0.1562500000001531830, 0.1718750000002726430, 0.1796875000003080869, 0.1835937500003257672, 0.1875000000003434752, 0.2187500000002969291, 0.2343750000002473299, 0.2421875000001830203, 0.2460937500001633693, 0.2500000000001437184, 0.2656250000001137979, 0.2812500000000838773, 0.2968750000000539013, 0.3046875000000662248, 0.3125000000000784928, 0.3437500000001323386, 0.3593750000001595946, 0.3671875000002268741, 0.3750000000002942091, 0.4062500000004605760, 0.4375000000006269429, 0.5000000000010219603, 0.5312500000012198020, 0.5625000000014177548, 0.5937500000016155965, 0.6093750000017141844, 0.6171875000017874591, 0.6250000000018607338, 0.6562500000022088997, 0.6718750000024367175, 0.6796875000025764946, 0.6835937500026186830, 0.6855468750026141311, 0.6875000000026094682, 0.7031250000027079450, 0.7109375000027615688, 0.7148437500027633451, 0.7187500000027652325, 0.7343750000026652014, 0.7421875000025792701, 0.7500000000024933389, 0.7812500000021941338, 0.7968750000020254909, 0.8046875000019169111, 0.8085937500018625101, 0.8125000000018082202, 0.8750000000012380097, 1.000000000000000000 ),
 .UNSPECIFIED. ) ;
#4261 = DIRECTION ( 'NONE',  ( -0.5000000000043351989, -0.8660254037819355988, 0.000000000000000000 ) ) ;
#4262 = CALENDAR_DATE ( 2026, 26, 10 ) ;
#4263 = EDGE_CURVE ( 'NONE', #21351, #12349, #2603, .T. ) ;
#4264 = ADVANCED_FACE ( 'NONE', ( #20044 ), #15712, .T. ) ;
#4265 = FACE_OUTER_BOUND ( 'NONE', #6709, .T. ) ;
#4266 = DIRECTION ( 'NONE',  ( -1.000000000000000000, 0.000000000000000000, 0.000000000000000000 ) ) ;
#4267 = DIRECTION ( 'NONE',  ( 0.000000000000000000, 1.000000000000000000, 0.000000000000000000 ) ) ;
#4268 = ADVANCED_FACE ( 'NONE', ( #5754 ), #21790, .F. ) ;
#4269 = VERTEX_POINT ( 'NONE', #6093 ) ;
#4270 = CIRCLE ( 'NONE', #11012, 4.114799999999974034 ) ;
#4271 = CARTESIAN_POINT ( 'NONE',  ( -6.349999999999999645, -3663.315000000000509, 2247.392000000000280 ) ) ;
#4272 = CIRCLE ( 'NONE', #17354, 2.844799999999009010 ) ;
#4273 = LINE ( 'NONE', #9662, #12167 ) ;
#4274 = ORIENTED_EDGE ( 'NONE', *, *, #3061, .F. ) ;
#4275 = EDGE_CURVE ( 'NONE', #6642, #15313, #11238, .T. ) ;
#4276 = DIRECTION ( 'NONE',  ( 0.000000000000000000, -0.8660254037817188832, 0.5000000000047110094 ) ) ;
#4277 = EDGE_LOOP ( 'NONE', ( #4388, #19502 ) ) ;
#4278 = EDGE_CURVE ( 'NONE', #13523, #8067, #18384, .T. ) ;
#4279 = DIRECTION ( 'NONE',  ( 0.000000000000000000, 0.000000000000000000, -1.000000000000000000 ) ) ;
#4280 = ORIENTED_EDGE ( 'NONE', *, *, #18670, .T. ) ;
#4281 = VERTEX_POINT ( 'NONE', #20370 ) ;
#4282 = DIRECTION ( 'NONE',  ( 1.000000000000000000, 0.000000000000000000, 0.000000000000000000 ) ) ;
#4283 = DIRECTION ( 'NONE',  ( 0.8660254037822586737, -0.5000000000037757575, 0.000000000000000000 ) ) ;
#4284 = CARTESIAN_POINT ( 'NONE',  ( 12.69999999999999929, -3648.710000000000036, 2268.705139999999574 ) ) ;
#4285 = CYLINDRICAL_SURFACE ( 'NONE', #8576, 2.844799999999994444 ) ;
#4286 = FACE_OUTER_BOUND ( 'NONE', #12773, .T. ) ;
#4287 = FACE_BOUND ( 'NONE', #18594, .T. ) ;
#4288 = AXIS2_PLACEMENT_3D ( 'NONE', #2648, #22436, #7933 ) ;
#4289 = DIRECTION ( 'NONE',  ( 0.000000000000000000, 0.000000000000000000, 1.000000000000000000 ) ) ;
#4290 = ORIENTED_EDGE ( 'NONE', *, *, #17425, .T. ) ;
#4291 = DATE_TIME_ROLE ( 'classification_date' ) ;
#4292 = AXIS2_PLACEMENT_3D ( 'NONE', #5882, #11361, #11142 ) ;
#4293 = EDGE_CURVE ( 'NONE', #20781, #10638, #21906, .T. ) ;
#4294 = CIRCLE ( 'NONE', #9895, 3.175000000000149925 ) ;
#4295 = CARTESIAN_POINT ( 'NONE',  ( 145.0394780070161005, -3657.466321062724546, 2246.411837555674538 ) ) ;
#4296 = DIRECTION ( 'NONE',  ( 1.000000000000000000, 0.000000000000000000, 0.000000000000000000 ) ) ;
#4297 = CARTESIAN_POINT ( 'NONE',  ( 17.78000000000000114, -3599.497499999999945, 2290.622800000000097 ) ) ;
#4298 = ORIENTED_EDGE ( 'NONE', *, *, #19987, .F. ) ;
#4299 = FACE_OUTER_BOUND ( 'NONE', #20323, .T. ) ;
#4300 = AXIS2_PLACEMENT_3D ( 'NONE', #4844, #12235, #19382 ) ;
#4301 = CARTESIAN_POINT ( 'NONE',  ( 111.4552000000009997, -3594.099999999999909, 2239.771999999999935 ) ) ;
#4302 = B_SPLINE_CURVE_WITH_KNOTS ( 'NONE', 3,
 ( #13606, #14914, #6008, #20625, #9737, #13141, #20514, #18752, #20748, #826, #20298, #4693, #22262, #18874, #9511, #11380, #6124, #18528, #4461, #18417, #4355, #2701, #13251 ),
 .UNSPECIFIED., .F., .F.,
 ( 4, 2, 2, 1, 1, 2, 2, 2, 2, 1, 2, 2, 4 ),
 ( 0.000000000000000000, 0.1250000000057876759, 0.1875000000086804175, 0.2187500000100172926, 0.2343750000102403086, 0.2421875000102004238, 0.2500000000101605391, 0.3750000000068593464, 0.4375000000056980531, 0.4687500000047965520, 0.4843750000046709858, 0.5000000000045454751, 1.000000000000000000 ),
 .UNSPECIFIED. ) ;
#4303 = ORIENTED_EDGE ( 'NONE', *, *, #17422, .T. ) ;
#4304 = DIRECTION ( 'NONE',  ( 5.155718784295149174E-12, -0.5000000000033149039, 0.8660254037825247941 ) ) ;
#4305 = AXIS2_PLACEMENT_3D ( 'NONE', #71, #23136, #9211 ) ;
#4306 = CARTESIAN_POINT ( 'NONE',  ( 13.66119911539924026, -3662.182772986108375, 2249.372110354217966 ) ) ;
#4307 = TOROIDAL_SURFACE ( 'NONE', #7307, 5.080000000000000071, 0.3810000000000000053 ) ;
#4308 = CARTESIAN_POINT ( 'NONE',  ( 12.69999999999999929, -3590.289999999999964, 2275.055139999999483 ) ) ;
#4309 = AXIS2_PLACEMENT_3D ( 'NONE', #18288, #4000, #9498 ) ;
#4310 = ORIENTED_EDGE ( 'NONE', *, *, #1052, .T. ) ;
#4311 = DIRECTION ( 'NONE',  ( 0.000000000000000000, 1.000000000000000000, 0.000000000000000000 ) ) ;
#4312 = CARTESIAN_POINT ( 'NONE',  ( 19.05000000000000071, -3578.860000000000127, 2247.392000000000280 ) ) ;
#4313 = CYLINDRICAL_SURFACE ( 'NONE', #20920, 2.844799999998995244 ) ;
#4314 = CARTESIAN_POINT ( 'NONE',  ( 60.73942059830999796, -3694.938000000000102, 2279.618249568000010 ) ) ;
#4315 = EDGE_LOOP ( 'NONE', ( #16089, #3871, #9853, #19218 ) ) ;
#4316 = ORIENTED_EDGE ( 'NONE', *, *, #17727, .F. ) ;
#4317 = PLANE ( 'NONE',  #6095 ) ;
#4318 = AXIS2_PLACEMENT_3D ( 'NONE', #11732, #5909, #16779 ) ;
#4319 = ORIENTED_EDGE ( 'NONE', *, *, #20548, .T. ) ;
#4320 = CARTESIAN_POINT ( 'NONE',  ( 142.5447999999989861, -3659.504999999999654, 2257.962944264955695 ) ) ;
#4321 = COORDINATED_UNIVERSAL_TIME_OFFSET ( 0, 0, .AHEAD. ) ;
#4322 = APPROVAL ( #18383, 'UNKNOWN' ) ;
#4323 = CIRCLE ( 'NONE', #2454, 2.844799999998998796 ) ;
#4324 = CARTESIAN_POINT ( 'NONE',  ( 145.3852444848333789, -3578.912497749951399, 2244.547653759440436 ) ) ;
#4325 = DIRECTION ( 'NONE',  ( -1.000000000000000000, 0.000000000000000000, 0.000000000000000000 ) ) ;
#4326 = AXIS2_PLACEMENT_3D ( 'NONE', #15834, #10670, #17818 ) ;
#4327 = CARTESIAN_POINT ( 'NONE',  ( 15.54479972194844528, -3579.494995305039538, 2257.962943247996918 ) ) ;
#4328 = DIRECTION ( 'NONE',  ( 0.000000000000000000, -1.000000000000000000, 0.000000000000000000 ) ) ;
#4329 = ADVANCED_FACE ( 'NONE', ( #13222 ), #14600, .T. ) ;
#4330 = CARTESIAN_POINT ( 'NONE',  ( 50.79999999999999716, -3619.500000000000000, 2239.009999999999764 ) ) ;
#4331 = ORIENTED_EDGE ( 'NONE', *, *, #3261, .T. ) ;
#4332 = DIRECTION ( 'NONE',  ( 0.000000000000000000, 0.000000000000000000, -1.000000000000000000 ) ) ;
#4333 = CARTESIAN_POINT ( 'NONE',  ( 7.619999999999999218, -3639.502500000000055, 2290.241799999999785 ) ) ;
#4334 = ORIENTED_EDGE ( 'NONE', *, *, #1942, .F. ) ;
#4335 = AXIS2_PLACEMENT_3D ( 'NONE', #14029, #10744, #8982 ) ;
#4336 = DIRECTION ( 'NONE',  ( -1.000000000000000000, 0.000000000000000000, 0.000000000000000000 ) ) ;
#4337 = CARTESIAN_POINT ( 'NONE',  ( 15.48293133199724103, -3543.482543407366393, 2255.165289490807481 ) ) ;
#4338 = TOROIDAL_SURFACE ( 'NONE', #11437, 7.112000000000000099, 0.7620000000000000107 ) ;
#4339 = ORIENTED_EDGE ( 'NONE', *, *, #22414, .F. ) ;
#4340 = CIRCLE ( 'NONE', #2470, 2.844800000000091700 ) ;
#4341 = ORIENTED_EDGE ( 'NONE', *, *, #11287, .F. ) ;
#4342 = EDGE_LOOP ( 'NONE', ( #21033, #12869 ) ) ;
#4343 = CARTESIAN_POINT ( 'NONE',  ( -12.69999999993336282, -3577.422685254774024, 2249.881502164204903 ) ) ;
#4344 = CIRCLE ( 'NONE', #11833, 3.606799999999001027 ) ;
#4345 = VERTEX_POINT ( 'NONE', #2115 ) ;
#4346 = CARTESIAN_POINT ( 'NONE',  ( -12.69999999999999929, -3577.293829546999859, 2244.679313203000220 ) ) ;
#4347 = CARTESIAN_POINT ( 'NONE',  ( 11.91900528410963211, -3576.759436215039386, 2249.310481143603283 ) ) ;
#4348 = CARTESIAN_POINT ( 'NONE',  ( 141.8830647757983741, -3581.319234992912698, 2248.822303562533762 ) ) ;
#4349 = ORIENTED_EDGE ( 'NONE', *, *, #944, .T. ) ;
#4350 = DIRECTION ( 'NONE',  ( 0.000000000000000000, 1.000000000000000000, 0.000000000000000000 ) ) ;
#4351 = PERSON_AND_ORGANIZATION ( #5446, #1895 ) ;
#4352 = APPROVAL ( #6170, 'UNSPECIFIED' ) ;
#4353 = DIRECTION ( 'NONE',  ( -1.224646799147353207E-16, 1.000000000000000000, 0.000000000000000000 ) ) ;
#4354 = AXIS2_PLACEMENT_3D ( 'NONE', #23126, #6986, #8736 ) ;
#4355 = CARTESIAN_POINT ( 'NONE',  ( 20.42964990730697039, -3543.731305792769490, 2260.325288752524102 ) ) ;
#4356 = AXIS2_PLACEMENT_3D ( 'NONE', #2073, #10971, #80 ) ;
#4357 = DIRECTION ( 'NONE',  ( -2.324635735433000053E-14, 0.000000000000000000, -1.000000000000000000 ) ) ;
#4358 = CIRCLE ( 'NONE', #19331, 6.477000000000000313 ) ;
#4359 = EDGE_CURVE ( 'NONE', #17172, #13234, #13100, .T. ) ;
#4360 = EDGE_CURVE ( 'NONE', #17332, #819, #7213, .T. ) ;
#4361 = B_SPLINE_CURVE_WITH_KNOTS ( 'NONE', 3,
 ( #10940, #169, #7318, #17859 ),
 .UNSPECIFIED., .F., .F.,
 ( 4, 4 ),
 ( 0.000000000000000000, 1.000000000000000000 ),
 .UNSPECIFIED. ) ;
#4362 = ORIENTED_EDGE ( 'NONE', *, *, #2300, .F. ) ;
#4363 = CARTESIAN_POINT ( 'NONE',  ( 15.03168679714000078, -3638.156300000000101, 2292.781800000000203 ) ) ;
#4364 = EDGE_CURVE ( 'NONE', #5314, #15707, #11132, .T. ) ;
#4365 = ORIENTED_EDGE ( 'NONE', *, *, #14237, .T. ) ;
#4366 = ORIENTED_EDGE ( 'NONE', *, *, #6966, .F. ) ;
#4367 = ORIENTED_EDGE ( 'NONE', *, *, #10353, .T. ) ;
#4368 = ORIENTED_EDGE ( 'NONE', *, *, #7698, .F. ) ;
#4369 = CARTESIAN_POINT ( 'NONE',  ( 142.0316867971999955, -3575.456400000000031, 2242.820000000000164 ) ) ;
#4370 = CARTESIAN_POINT ( 'NONE',  ( 139.6999999999999886, -3659.504999999999654, 2239.771999999999935 ) ) ;
#4371 = EDGE_CURVE ( 'NONE', #20621, #9389, #9974, .T. ) ;
#4372 = ORIENTED_EDGE ( 'NONE', *, *, #12695, .T. ) ;
#4373 = VECTOR ( 'NONE', #962, 1000.000000000000000 ) ;
#4374 = DIRECTION ( 'NONE',  ( 0.8660254037822586737, -0.5000000000037757575, 0.000000000000000000 ) ) ;
#4375 = DIRECTION ( 'NONE',  ( -1.000000000000000000, 0.000000000000000000, 0.000000000000000000 ) ) ;
#4376 = EDGE_CURVE ( 'NONE', #3687, #18263, #2990, .T. ) ;
#4377 = CIRCLE ( 'NONE', #2866, 1.904999999999823501 ) ;
#4378 = CARTESIAN_POINT ( 'NONE',  ( -5.588000000000000078, -3543.299999999999727, 2229.612000000000080 ) ) ;
#4379 = PERSON_AND_ORGANIZATION ( #5446, #1895 ) ;
#4380 = CARTESIAN_POINT ( 'NONE',  ( 12.69999999999999929, -3579.494999999999891, 2272.030000000000200 ) ) ;
#4381 = DIRECTION ( 'NONE',  ( 0.000000000000000000, 0.000000000000000000, -1.000000000000000000 ) ) ;
#4382 = CARTESIAN_POINT ( 'NONE',  ( 144.7800000000000011, -3659.504999999999654, 2239.391000000000076 ) ) ;
#4383 = ORIENTED_EDGE ( 'NONE', *, *, #11771, .T. ) ;
#4384 = CARTESIAN_POINT ( 'NONE',  ( 136.8622934043370094, -3543.413280444360680, 2255.028323493608241 ) ) ;
#4385 = EDGE_CURVE ( 'NONE', #21408, #11171, #12346, .T. ) ;
#4386 = VECTOR ( 'NONE', #22835, 1000.000000000000114 ) ;
#4387 = DIRECTION ( 'NONE',  ( 0.000000000000000000, 0.000000000000000000, -1.000000000000000000 ) ) ;
#4388 = ORIENTED_EDGE ( 'NONE', *, *, #19258, .F. ) ;
#4389 = CARTESIAN_POINT ( 'NONE',  ( 140.9635494321942417, -3582.050586540670338, 2257.663356974309863 ) ) ;
#4390 = ADVANCED_FACE ( 'NONE', ( #18718 ), #17195, .F. ) ;
#4391 = CIRCLE ( 'NONE', #5915, 5.460999999999938126 ) ;
#4392 = ADVANCED_FACE ( 'NONE', ( #6203 ), #15339, .T. ) ;
#4393 = PLANE ( 'NONE',  #2469 ) ;
#4394 = VECTOR ( 'NONE', #1166, 1000.000000000000114 ) ;
#4395 = ORIENTED_EDGE ( 'NONE', *, *, #17604, .T. ) ;
#4396 = ORIENTED_EDGE ( 'NONE', *, *, #8889, .F. ) ;
#4397 = DIRECTION ( 'NONE',  ( -2.330758767202000237E-14, -1.000000000000000000, -1.224646799141892318E-16 ) ) ;
#4398 = AXIS2_PLACEMENT_3D ( 'NONE', #5164, #17213, #3389 ) ;
#4399 = CARTESIAN_POINT ( 'NONE',  ( 9.524999999998000177, -3543.299999999999727, 2281.351799999999912 ) ) ;
#4400 = CARTESIAN_POINT ( 'NONE',  ( 22.76381536726000121, -3694.938000000000102, 2275.540615367000555 ) ) ;
#4401 = DIRECTION ( 'NONE',  ( 1.000000000000000000, 0.000000000000000000, 0.000000000000000000 ) ) ;
#4402 = CARTESIAN_POINT ( 'NONE',  ( 73.35520000000001062, -3670.300000000000182, 2259.837999999999738 ) ) ;
#4403 = CARTESIAN_POINT ( 'NONE',  ( 2.859369265602505816, -3543.299999999999727, 2275.763800000000629 ) ) ;
#4404 = ORIENTED_EDGE ( 'NONE', *, *, #17016, .T. ) ;
#4405 = PERSON_AND_ORGANIZATION ( #5446, #1895 ) ;
#4406 = AXIS2_PLACEMENT_3D ( 'NONE', #11623, #1079, #13627 ) ;
#4407 = CARTESIAN_POINT ( 'NONE',  ( 21.79320000000099711, -3619.500000000000000, 2260.600000000000364 ) ) ;
#4408 = EDGE_CURVE ( 'NONE', #7794, #15892, #8973, .T. ) ;
#4409 = VECTOR ( 'NONE', #20650, 1000.000000000000000 ) ;
#4410 = CARTESIAN_POINT ( 'NONE',  ( 12.69999999999999929, -3659.504999999999654, 2272.030000000000200 ) ) ;
#4411 = DIRECTION ( 'NONE',  ( 0.000000000000000000, 0.000000000000000000, 1.000000000000000000 ) ) ;
#4412 = ORIENTED_EDGE ( 'NONE', *, *, #5876, .T. ) ;
#4413 = LINE ( 'NONE', #17395, #12601 ) ;
#4414 = PLANE ( 'NONE',  #19629 ) ;
#4415 = CARTESIAN_POINT ( 'NONE',  ( 134.9433685273030221, -3576.326160261962286, 2246.096241041220765 ) ) ;
#4416 = VERTEX_POINT ( 'NONE', #22582 ) ;
#4417 = DIRECTION ( 'NONE',  ( 0.000000000000000000, 0.000000000000000000, 1.000000000000000000 ) ) ;
#4418 = CARTESIAN_POINT ( 'NONE',  ( 15.28666681192564525, -3660.698594568427779, 2250.184763937277239 ) ) ;
#4419 = CIRCLE ( 'NONE', #11521, 3.606799999998994366 ) ;
#4420 = ADVANCED_FACE ( 'NONE', ( #15219 ), #17947, .T. ) ;
#4421 = CARTESIAN_POINT ( 'NONE',  ( 20.32000000000000028, -3544.061999999999898, 2289.213099999999940 ) ) ;
#4422 = ORIENTED_EDGE ( 'NONE', *, *, #19679, .T. ) ;
#4423 = ORIENTED_EDGE ( 'NONE', *, *, #12597, .F. ) ;
#4424 = DIRECTION ( 'NONE',  ( -0.8660254037815640071, 0.5000000000049790172, 0.000000000000000000 ) ) ;
#4425 = B_SPLINE_CURVE_WITH_KNOTS ( 'NONE', 3,
 ( #5899, #13036, #11267, #18414 ),
 .UNSPECIFIED., .F., .F.,
 ( 4, 4 ),
 ( 0.000000000000000000, 3.168591426078622932E-06 ),
 .UNSPECIFIED. ) ;
#4426 = DIRECTION ( 'NONE',  ( 0.000000000000000000, 0.000000000000000000, 1.000000000000000000 ) ) ;
#4427 = FACE_BOUND ( 'NONE', #1511, .T. ) ;
#4428 = DIRECTION ( 'NONE',  ( 0.000000000000000000, -1.000000000000000000, 0.000000000000000000 ) ) ;
#4429 = ORIENTED_EDGE ( 'NONE', *, *, #14013, .F. ) ;
#4430 = FACE_OUTER_BOUND ( 'NONE', #432, .T. ) ;
#4431 = ORIENTED_EDGE ( 'NONE', *, *, #10605, .T. ) ;
#4432 = EDGE_CURVE ( 'NONE', #5265, #833, #13114, .T. ) ;
#4433 = CARTESIAN_POINT ( 'NONE',  ( 145.2640895604332911, -3580.799603742848831, 2245.310931595014154 ) ) ;
#4434 = COORDINATED_UNIVERSAL_TIME_OFFSET ( 0, 0, .AHEAD. ) ;
#4435 = EDGE_CURVE ( 'NONE', #17227, #15832, #11929, .T. ) ;
#4436 = CARTESIAN_POINT ( 'NONE',  ( 141.1353819521796709, -3577.011135563875087, 2257.680384088092524 ) ) ;
#4437 = CARTESIAN_POINT ( 'NONE',  ( 18.29809890354264112, -3660.655555570265278, 2244.593310214874236 ) ) ;
#4438 = AXIS2_PLACEMENT_3D ( 'NONE', #15437, #12034, #19305 ) ;
#4439 = FACE_OUTER_BOUND ( 'NONE', #20191, .T. ) ;
#4440 = DIRECTION ( 'NONE',  ( 0.5000000000031885605, -0.8660254037825977358, 0.000000000000000000 ) ) ;
#4441 = DIRECTION ( 'NONE',  ( -1.000000000000000000, 0.000000000000000000, 0.000000000000000000 ) ) ;
#4442 = ORIENTED_EDGE ( 'NONE', *, *, #14855, .F. ) ;
#4443 = CARTESIAN_POINT ( 'NONE',  ( 12.69999999999999929, -3599.497499999999945, 2263.571799999999712 ) ) ;
#4444 = EDGE_LOOP ( 'NONE', ( #282, #12706, #8347, #4918 ) ) ;
#4445 = FACE_OUTER_BOUND ( 'NONE', #18036, .T. ) ;
#4446 = DIRECTION ( 'NONE',  ( 0.000000000000000000, -1.000000000000000000, 0.000000000000000000 ) ) ;
#4447 = ORIENTED_EDGE ( 'NONE', *, *, #15005, .F. ) ;
#4448 = ORIENTED_EDGE ( 'NONE', *, *, #10833, .T. ) ;
#4449 = ORIENTED_EDGE ( 'NONE', *, *, #2579, .T. ) ;
#4450 = CARTESIAN_POINT ( 'NONE',  ( -12.31900000000012696, -3584.320999999999913, 2247.392000000000280 ) ) ;
#4451 = CIRCLE ( 'NONE', #12691, 5.460999999999938126 ) ;
#4452 = VERTEX_POINT ( 'NONE', #8419 ) ;
#4453 = DIRECTION ( 'NONE',  ( 0.000000000000000000, 0.000000000000000000, 1.000000000000000000 ) ) ;
#4454 = CARTESIAN_POINT ( 'NONE',  ( 11.26161571375768133, -3577.038842554089115, 2249.578370015894961 ) ) ;
#4455 = APPLICATION_PROTOCOL_DEFINITION ( 'international standard', 'automotive_design', 2000, #6788 ) ;
#4456 = CARTESIAN_POINT ( 'NONE',  ( 19.05000000000000071, -3575.684999999999945, 2247.392000000000280 ) ) ;
#4457 = VERTEX_POINT ( 'NONE', #13813 ) ;
#4458 = CARTESIAN_POINT ( 'NONE',  ( 0.7620000000000000107, -3694.938000000000102, 2239.771999999999935 ) ) ;
#4459 = COORDINATED_UNIVERSAL_TIME_OFFSET ( 0, 0, .AHEAD. ) ;
#4460 = DIRECTION ( 'NONE',  ( -0.8660254037821902839, 0.5000000000038942183, 1.814359422184980810E-12 ) ) ;
#4461 = CARTESIAN_POINT ( 'NONE',  ( 20.52512745630702184, -3543.549679414229558, 2260.086245106032948 ) ) ;
#4462 = AXIS2_PLACEMENT_3D ( 'NONE', #7470, #18129, #2088 ) ;
#4463 = CARTESIAN_POINT ( 'NONE',  ( 136.9269754645999910, -3578.860002036999958, 2250.236803302000226 ) ) ;
#4464 = VERTEX_POINT ( 'NONE', #13575 ) ;
#4465 = CARTESIAN_POINT ( 'NONE',  ( 116.8400000000002734, -3670.300000000000182, 2244.547199999999975 ) ) ;
#4466 = ORIENTED_EDGE ( 'NONE', *, *, #10291, .F. ) ;
#4467 = VERTEX_POINT ( 'NONE', #20955 ) ;
#4468 = ORIENTED_EDGE ( 'NONE', *, *, #2834, .T. ) ;
#4469 = APPLIED_PERSON_AND_ORGANIZATION_ASSIGNMENT ( #18894, #15274, ( #10138 ) ) ;
#4470 = DIRECTION ( 'NONE',  ( 0.000000000000000000, 0.000000000000000000, 1.000000000000000000 ) ) ;
#4471 = EDGE_LOOP ( 'NONE', ( #4404, #20592 ) ) ;
#4472 = FACE_OUTER_BOUND ( 'NONE', #1916, .T. ) ;
#4473 = CARTESIAN_POINT ( 'NONE',  ( 67.10679999999999268, -3644.899999999999636, 2259.837999999999738 ) ) ;
#4474 = AXIS2_PLACEMENT_3D ( 'NONE', #6, #10429, #15940 ) ;
#4475 = ORIENTED_EDGE ( 'NONE', *, *, #7426, .F. ) ;
#4476 = CARTESIAN_POINT ( 'NONE',  ( 0.000000000000000000, -3694.430000000000291, 2254.503999999999905 ) ) ;
#4477 = ADVANCED_FACE ( 'NONE', ( #9816 ), #8304, .F. ) ;
#4478 = CARTESIAN_POINT ( 'NONE',  ( 139.6999999999999886, -3579.494999999999891, 2245.359999999999673 ) ) ;
#4479 = APPLIED_APPROVAL_ASSIGNMENT ( #12204, ( #6739 ) ) ;
#4480 = ADVANCED_FACE ( 'NONE', ( #1024 ), #18842, .T. ) ;
#4481 =( GEOMETRIC_REPRESENTATION_CONTEXT ( 3 ) GLOBAL_UNCERTAINTY_ASSIGNED_CONTEXT ( ( #17837 ) ) GLOBAL_UNIT_ASSIGNED_CONTEXT ( ( #13621, #15622, #17129 ) ) REPRESENTATION_CONTEXT ( 'NONE', 'WORKASPACE' ) );
#4482 = DIRECTION ( 'NONE',  ( 1.000000000000000000, 0.000000000000000000, 0.000000000000000000 ) ) ;
#4483 = APPROVAL_DATE_TIME ( #518, #12070 ) ;
#4484 = EDGE_CURVE ( 'NONE', #21855, #10396, #19201, .T. ) ;
#4485 = LINE ( 'NONE', #5922, #22877 ) ;
#4486 = DIRECTION ( 'NONE',  ( 0.000000000000000000, 0.000000000000000000, -1.000000000000000000 ) ) ;
#4487 = LINE ( 'NONE', #22066, #22536 ) ;
#4488 = DIRECTION ( 'NONE',  ( 0.000000000000000000, 0.000000000000000000, -1.000000000000000000 ) ) ;
#4489 = EDGE_CURVE ( 'NONE', #15062, #4703, #11973, .T. ) ;
#4490 = ORIENTED_EDGE ( 'NONE', *, *, #18998, .T. ) ;
#4491 = CARTESIAN_POINT ( 'NONE',  ( 136.6529205195000145, -3543.299999999999727, 2254.503999999999905 ) ) ;
#4492 = VECTOR ( 'NONE', #12977, 999.9999999999998863 ) ;
#4493 = APPLIED_APPROVAL_ASSIGNMENT ( #11201, ( #8248 ) ) ;
#4494 = ADVANCED_FACE ( 'NONE', ( #8651 ), #15797, .F. ) ;
#4495 = SECURITY_CLASSIFICATION ( '', '', #5949 ) ;
#4496 = EDGE_LOOP ( 'NONE', ( #20471, #13892, #2244, #17277 ) ) ;
#4497 = CARTESIAN_POINT ( 'NONE',  ( 141.1265829755976711, -3581.963233858874901, 2257.683488260704507 ) ) ;
#4498 = CARTESIAN_POINT ( 'NONE',  ( 18.37220258132071393, -3658.807050315976994, 2244.878795110561441 ) ) ;
#4499 = ORIENTED_EDGE ( 'NONE', *, *, #13499, .T. ) ;
#4500 = ORIENTED_EDGE ( 'NONE', *, *, #11923, .T. ) ;
#4501 = DIRECTION ( 'NONE',  ( 1.000000000000000000, 0.000000000000000000, 0.000000000000000000 ) ) ;
#4502 = FACE_OUTER_BOUND ( 'NONE', #6101, .T. ) ;
#4503 = CARTESIAN_POINT ( 'NONE',  ( 130.6067999999989979, -3619.500000000000000, 2259.837999999999738 ) ) ;
#4504 = CARTESIAN_POINT ( 'NONE',  ( 25.39999999999999858, -3660.140000000000327, 2250.236800000000130 ) ) ;
#4505 = B_SPLINE_CURVE_WITH_KNOTS ( 'NONE', 3,
 ( #9711, #16625, #16403, #20271, #20048, #583, #7736, #11351, #14654, #20376, #14888, #2565, #5874, #9266, #12889, #2118, #21795, #9603, #22017 ),
 .UNSPECIFIED., .F., .F.,
 ( 4, 1, 1, 1, 1, 1, 1, 1, 1, 1, 1, 1, 1, 1, 1, 1, 4 ),
 ( 0.000000000000000000, 0.06250000000000000000, 0.1250000000000000000, 0.1875000000000000000, 0.2500000000000000000, 0.3125000000000000000, 0.3750000000000000000, 0.4375000000000000000, 0.5000000000000000000, 0.5625000000000000000, 0.6250000000000000000, 0.6875000000000000000, 0.7500000000000000000, 0.8125000000000000000, 0.8750000000000000000, 0.9375000000000000000, 1.000000000000000000 ),
 .UNSPECIFIED. ) ;
#4506 = CARTESIAN_POINT ( 'NONE',  ( 136.9475605302572490, -3658.761901444864179, 2257.938841409468296 ) ) ;
#4507 = DIRECTION ( 'NONE',  ( 0.7071067811865969777, 0.000000000000000000, -0.7071067811864980568 ) ) ;
#4508 = EDGE_CURVE ( 'NONE', #10059, #19085, #22071, .T. ) ;
#4509 = ORIENTED_EDGE ( 'NONE', *, *, #22542, .F. ) ;
#4510 = SECURITY_CLASSIFICATION_LEVEL ( 'unclassified' ) ;
#4511 = EDGE_CURVE ( 'NONE', #8413, #3889, #6339, .T. ) ;
#4512 = ORIENTED_EDGE ( 'NONE', *, *, #2138, .T. ) ;
#4513 = DIRECTION ( 'NONE',  ( 0.000000000000000000, 0.000000000000000000, 1.000000000000000000 ) ) ;
#4514 = APPROVAL_PERSON_ORGANIZATION ( #16215, #15483, #12590 ) ;
#4515 = LOCAL_TIME ( 17, 37, 43.00000000000000000, #20800 ) ;
#4516 = DIRECTION ( 'NONE',  ( 0.000000000000000000, 0.000000000000000000, 1.000000000000000000 ) ) ;
#4517 = CARTESIAN_POINT ( 'NONE',  ( 10.36831320285999958, -3658.158799999999701, 2239.391000000000076 ) ) ;
#4518 = ORIENTED_EDGE ( 'NONE', *, *, #17655, .T. ) ;
#4519 = DIRECTION ( 'NONE',  ( 0.000000000000000000, 0.000000000000000000, -1.000000000000000000 ) ) ;
#4520 = AXIS2_PLACEMENT_3D ( 'NONE', #2297, #14842, #3813 ) ;
#4521 = EDGE_CURVE ( 'NONE', #19192, #10469, #17589, .T. ) ;
#4522 = FACE_OUTER_BOUND ( 'NONE', #16707, .T. ) ;
#4523 = CARTESIAN_POINT ( 'NONE',  ( 144.9020910522499435, -3661.871258547513662, 2245.134603803046048 ) ) ;
#4524 = EDGE_LOOP ( 'NONE', ( #21514, #20558, #5691, #9992 ) ) ;
#4525 = DIRECTION ( 'NONE',  ( 1.000000000000000000, 0.000000000000000000, 0.000000000000000000 ) ) ;
#4526 = CARTESIAN_POINT ( 'NONE',  ( 15.47291618100999955, -3660.140271294999820, 2250.236802488000194 ) ) ;
#4527 = CARTESIAN_POINT ( 'NONE',  ( -12.31900000000000084, -3661.486200000121244, 2249.723686796789480 ) ) ;
#4528 = ORIENTED_EDGE ( 'NONE', *, *, #17738, .F. ) ;
#4529 = B_SPLINE_CURVE_WITH_KNOTS ( 'NONE', 3,
 ( #21356, #6718, #19475, #12212 ),
 .UNSPECIFIED., .F., .F.,
 ( 4, 4 ),
 ( 0.000000000000000000, 1.000000000000000000 ),
 .UNSPECIFIED. ) ;
#4530 = CYLINDRICAL_SURFACE ( 'NONE', #9556, 2.844800000000001550 ) ;
#4531 = FACE_OUTER_BOUND ( 'NONE', #11288, .T. ) ;
#4532 = DIRECTION ( 'NONE',  ( 0.000000000000000000, 0.000000000000000000, -1.000000000000000000 ) ) ;
#4533 = CARTESIAN_POINT ( 'NONE',  ( 35.56000000000000227, -3670.300000000000182, 2250.236800000000130 ) ) ;
#4534 = DIRECTION ( 'NONE',  ( -1.000000000000000000, 0.000000000000000000, 0.000000000000000000 ) ) ;
#4535 = AXIS2_PLACEMENT_3D ( 'NONE', #10251, #20680, #3226 ) ;
#4536 = ORIENTED_EDGE ( 'NONE', *, *, #18405, .F. ) ;
#4537 = VECTOR ( 'NONE', #17008, 1000.000000000000000 ) ;
#4538 = ORIENTED_EDGE ( 'NONE', *, *, #9152, .F. ) ;
#4539 = CARTESIAN_POINT ( 'NONE',  ( 141.8426865358000271, -3657.624611564246152, 2257.800363195205136 ) ) ;
#4540 = PERSON_AND_ORGANIZATION ( #7393, #11600 ) ;
#4541 = EDGE_CURVE ( 'NONE', #10440, #4464, #1874, .T. ) ;
#4542 = EDGE_CURVE ( 'NONE', #9572, #12083, #6754, .T. ) ;
#4543 = CARTESIAN_POINT ( 'NONE',  ( 18.21995551375025357, -3660.985253975473825, 2244.675656256517868 ) ) ;
#4544 = CARTESIAN_POINT ( 'NONE',  ( 14.27729191008000065, -3657.131900051000230, 2257.704292951999832 ) ) ;
#4545 = CARTESIAN_POINT ( 'NONE',  ( 57.14999999999999858, -3695.699999999999818, 2247.392000000000280 ) ) ;
#4546 = DIRECTION ( 'NONE',  ( 0.000000000000000000, -1.000000000000000000, 0.000000000000000000 ) ) ;
#4547 = EDGE_CURVE ( 'NONE', #9227, #8952, #12737, .T. ) ;
#4548 = ORIENTED_EDGE ( 'NONE', *, *, #13941, .F. ) ;
#4549 = CIRCLE ( 'NONE', #1939, 2.844800000000091700 ) ;
#4550 = DIRECTION ( 'NONE',  ( -2.324635735433000053E-14, 2.336881798971000105E-14, -1.000000000000000000 ) ) ;
#4551 = AXIS2_PLACEMENT_3D ( 'NONE', #11588, #9497, #8093 ) ;
#4552 = EDGE_LOOP ( 'NONE', ( #10248, #7218 ) ) ;
#4553 = DIRECTION ( 'NONE',  ( 0.6723379328173905156, 0.7402443543147344540, 0.000000000000000000 ) ) ;
#4554 = CARTESIAN_POINT ( 'NONE',  ( 10.76878381091101389, -3657.415877871818793, 2248.216115161493235 ) ) ;
#4555 = EDGE_CURVE ( 'NONE', #19652, #2680, #14619, .T. ) ;
#4556 = VERTEX_POINT ( 'NONE', #10521 ) ;
#4557 = VERTEX_POINT ( 'NONE', #19319 ) ;
#4558 = ADVANCED_FACE ( 'NONE', ( #21312 ), #16478, .T. ) ;
#4559 = VERTEX_POINT ( 'NONE', #3713 ) ;
#4560 = ORIENTED_EDGE ( 'NONE', *, *, #13323, .T. ) ;
#4561 = APPROVAL_STATUS ( 'not_yet_approved' ) ;
#4562 = DIRECTION ( 'NONE',  ( 2.336881798971000105E-14, 2.336881798971000105E-14, 1.000000000000000000 ) ) ;
#4563 = PRODUCT_DEFINITION_CONTEXT ( 'detailed design', #12493, 'design' ) ;
#4564 =( BOUNDED_CURVE ( )  B_SPLINE_CURVE ( 3, ( #22848, #6820, #3292, #1532 ),
 .UNSPECIFIED., .F., .F. ) 
 B_SPLINE_CURVE_WITH_KNOTS ( ( 4, 4 ),
 ( 1.570796327718551932, 3.141592653590084883 ),
 .UNSPECIFIED. ) 
 CURVE ( )  GEOMETRIC_REPRESENTATION_ITEM ( )  RATIONAL_B_SPLINE_CURVE ( ( 1.000000000000000000, 0.8047378543420038444, 0.8047378543420038444, 1.000000000000000000 ) ) 
 REPRESENTATION_ITEM ( '' )  );
#4565 = AXIS2_PLACEMENT_3D ( 'NONE', #19402, #13897, #10139 ) ;
#4566 = ORIENTED_EDGE ( 'NONE', *, *, #17603, .F. ) ;
#4567 = CARTESIAN_POINT ( 'NONE',  ( 139.6999999999999886, -3659.504999999999654, 2272.030000000000200 ) ) ;
#4568 = DIRECTION ( 'NONE',  ( 1.224646799147353207E-16, 1.000000000000000000, -0.000000000000000000 ) ) ;
#4569 = CARTESIAN_POINT ( 'NONE',  ( 0.000000000000000000, 0.000000000000000000, 0.000000000000000000 ) ) ;
#4570 = CARTESIAN_POINT ( 'NONE',  ( 141.5925613388025397, -3581.618976631144051, 2248.085587691497039 ) ) ;
#4571 = AXIS2_PLACEMENT_3D ( 'NONE', #20864, #1281, #6580 ) ;
#4572 = EDGE_LOOP ( 'NONE', ( #19850, #22853, #13047, #14458 ) ) ;
#4573 = CARTESIAN_POINT ( 'NONE',  ( 137.2316812770350225, -3660.931433079190356, 2257.869726282126976 ) ) ;
#4574 = CALENDAR_DATE ( 2026, 26, 10 ) ;
#4575 = VECTOR ( 'NONE', #12036, 1000.000000000000000 ) ;
#4576 = EDGE_CURVE ( 'NONE', #14130, #12971, #8887, .T. ) ;
#4577 = DIRECTION ( 'NONE',  ( 1.000000000000000000, 0.000000000000000000, 0.000000000000000000 ) ) ;
#4578 = DIRECTION ( 'NONE',  ( -1.000000000000000000, 0.000000000000000000, 0.000000000000000000 ) ) ;
#4579 = CARTESIAN_POINT ( 'NONE',  ( 134.3272858694121510, -3657.550344535092336, 2246.178645530484573 ) ) ;
#4580 = ORIENTED_EDGE ( 'NONE', *, *, #12641, .F. ) ;
#4581 = AXIS2_PLACEMENT_3D ( 'NONE', #21935, #383, #5901 ) ;
#4582 = CARTESIAN_POINT ( 'NONE',  ( 12.69999999999999929, -3599.497499999999945, 2288.971800000000258 ) ) ;
#4583 = EDGE_LOOP ( 'NONE', ( #12321, #14783, #9126, #4412 ) ) ;
#4584 = ORIENTED_EDGE ( 'NONE', *, *, #2556, .F. ) ;
#4585 = CIRCLE ( 'NONE', #14342, 11.11250000000000071 ) ;
#4586 = CIRCLE ( 'NONE', #18443, 0.7620000000000000107 ) ;
#4587 = DIRECTION ( 'NONE',  ( 0.000000000000000000, 0.000000000000000000, -1.000000000000000000 ) ) ;
#4588 = ORIENTED_EDGE ( 'NONE', *, *, #16015, .T. ) ;
#4589 = ORIENTED_EDGE ( 'NONE', *, *, #2542, .F. ) ;
#4590 = DIRECTION ( 'NONE',  ( 0.000000000000000000, 1.000000000000000000, 0.000000000000000000 ) ) ;
#4591 = DIRECTION ( 'NONE',  ( 0.000000000000000000, 0.000000000000000000, -1.000000000000000000 ) ) ;
#4592 = ORIENTED_EDGE ( 'NONE', *, *, #2220, .T. ) ;
#4593 = CARTESIAN_POINT ( 'NONE',  ( 7.138340810734780995, -3658.190072843201960, 2245.320604752622785 ) ) ;
#4594 = SHAPE_REPRESENTATION_RELATIONSHIP ( 'NONE' , 'NONE' ,  #13255, #19426 ) ;
#4595 = DIRECTION ( 'NONE',  ( 2.848812946084999742E-12, 1.000000000000000000, -2.336881798978000141E-14 ) ) ;
#4596 = PERSON ( 'NAUO-PER14', 'UNSPECIFIED', 'UNSPECIFIED', ('UNSPECIFIED'), ('UNSPECIFIED'), ('UNSPECIFIED') ) ;
#4597 = DIRECTION ( 'NONE',  ( -1.000000000000000000, 0.000000000000000000, 0.000000000000000000 ) ) ;
#4598 = VECTOR ( 'NONE', #4212, 999.9999999999998863 ) ;
#4599 = DATE_TIME_ROLE ( 'classification_date' ) ;
#4600 = DIRECTION ( 'NONE',  ( 1.000000000000000000, 0.000000000000000000, 0.000000000000000000 ) ) ;
#4601 = DIRECTION ( 'NONE',  ( 0.000000000000000000, 0.000000000000000000, -1.000000000000000000 ) ) ;
#4602 = DIRECTION ( 'NONE',  ( 0.000000000000000000, -1.000000000000000000, 0.000000000000000000 ) ) ;
#4603 = AXIS2_PLACEMENT_3D ( 'NONE', #8502, #5574, #17868 ) ;
#4604 = APPLIED_PERSON_AND_ORGANIZATION_ASSIGNMENT ( #17919, #16168, ( #785 ) ) ;
#4605 = AXIS2_PLACEMENT_3D ( 'NONE', #19354, #1176, #3171 ) ;
#4606 = DIRECTION ( 'NONE',  ( 0.000000000000000000, 0.000000000000000000, 1.000000000000000000 ) ) ;
#4607 = CARTESIAN_POINT ( 'NONE',  ( 139.6999999999999886, -3659.504999999999654, 2245.359999999999673 ) ) ;
#4608 = VERTEX_POINT ( 'NONE', #8996 ) ;
#4609 = DIRECTION ( 'NONE',  ( 0.000000000000000000, -1.000000000000000000, 0.000000000000000000 ) ) ;
#4610 = EDGE_CURVE ( 'NONE', #1122, #8369, #16149, .T. ) ;
#4611 = ORIENTED_EDGE ( 'NONE', *, *, #3214, .T. ) ;
#4612 = AXIS2_PLACEMENT_3D ( 'NONE', #19323, #12833, #2057 ) ;
#4613 = FACE_OUTER_BOUND ( 'NONE', #2979, .T. ) ;
#4614 = EDGE_CURVE ( 'NONE', #444, #16167, #9005, .T. ) ;
#4615 = CARTESIAN_POINT ( 'NONE',  ( -5.588000000000000078, -3543.299999999999727, 2229.612000000000080 ) ) ;
#4616 = VERTEX_POINT ( 'NONE', #12634 ) ;
#4617 = ORIENTED_EDGE ( 'NONE', *, *, #6507, .T. ) ;
#4618 = DIRECTION ( 'NONE',  ( 0.000000000000000000, 0.000000000000000000, -1.000000000000000000 ) ) ;
#4619 = LINE ( 'NONE', #11533, #18487 ) ;
#4620 = CARTESIAN_POINT ( 'NONE',  ( 10.68406120964000117, -3601.513414593999642, 2279.634081700000479 ) ) ;
#4621 = ORIENTED_EDGE ( 'NONE', *, *, #10817, .F. ) ;
#4622 = CIRCLE ( 'NONE', #17719, 2.844799999998903761 ) ;
#4623 = DIRECTION ( 'NONE',  ( -1.000000000000000000, 0.000000000000000000, 0.000000000000000000 ) ) ;
#4624 = CARTESIAN_POINT ( 'NONE',  ( -8.890000000017000303, -3577.513800000000174, 2249.723686796999573 ) ) ;
#4625 = CARTESIAN_POINT ( 'NONE',  ( 151.1299999999999955, -3694.430000000000291, 2259.329999999999927 ) ) ;
#4626 = CARTESIAN_POINT ( 'NONE',  ( 20.67261935617544211, -3695.639689706588797, 2259.716784108924458 ) ) ;
#4627 = ORIENTED_EDGE ( 'NONE', *, *, #5455, .T. ) ;
#4628 = APPROVAL_ROLE ( '' ) ;
#4629 = ORIENTED_EDGE ( 'NONE', *, *, #18562, .T. ) ;
#4630 = APPROVAL ( #3101, 'UNSPECIFIED' ) ;
#4631 = CARTESIAN_POINT ( 'NONE',  ( 9.935234496185218589, -3580.171483082290251, 2249.918062184726750 ) ) ;
#4632 = FACE_OUTER_BOUND ( 'NONE', #9124, .T. ) ;
#4633 = VERTEX_POINT ( 'NONE', #18017 ) ;
#4634 = DIRECTION ( 'NONE',  ( -1.000000000000000000, 0.000000000000000000, 0.000000000000000000 ) ) ;
#4635 = EDGE_CURVE ( 'NONE', #2888, #17496, #1968, .T. ) ;
#4636 = CARTESIAN_POINT ( 'NONE',  ( 151.1299999999999955, -3660.140000000000327, 2250.236800000000130 ) ) ;
#4637 = CARTESIAN_POINT ( 'NONE',  ( 144.7317021135920356, -3662.214841093968516, 2245.445731933329625 ) ) ;
#4638 = ORIENTED_EDGE ( 'NONE', *, *, #20739, .F. ) ;
#4639 = EDGE_CURVE ( 'NONE', #10769, #10464, #667, .T. ) ;
#4640 = CARTESIAN_POINT ( 'NONE',  ( 13.81460452052465548, -3662.123667865505922, 2249.431728352276878 ) ) ;
#4641 = ADVANCED_FACE ( 'NONE', ( #22097 ), #14858, .F. ) ;
#4642 = DIRECTION ( 'NONE',  ( 0.8660254037842058938, 0.5000000000004030110, -5.443078266503040078E-12 ) ) ;
#4643 = ORIENTED_EDGE ( 'NONE', *, *, #14715, .T. ) ;
#4644 = CARTESIAN_POINT ( 'NONE',  ( -12.69999999999999929, -3577.293829546977122, 2244.679313203000220 ) ) ;
#4645 = TOROIDAL_SURFACE ( 'NONE', #3158, 3.606799999999999784, 0.7620000000000000107 ) ;
#4646 = CARTESIAN_POINT ( 'NONE',  ( 114.2999999999999972, -3644.899999999999636, 2260.600000000000364 ) ) ;
#4647 = CIRCLE ( 'NONE', #2825, 2.844799999998995244 ) ;
#4648 = FACE_OUTER_BOUND ( 'NONE', #15083, .T. ) ;
#4649 = CIRCLE ( 'NONE', #13636, 2.844799999999999773 ) ;
#4650 = DIRECTION ( 'NONE',  ( -1.000000000000000000, 0.000000000000000000, 0.000000000000000000 ) ) ;
#4651 = CARTESIAN_POINT ( 'NONE',  ( 3.810000000000000053, -3543.299999999999727, 2239.009999999999764 ) ) ;
#4652 = EDGE_LOOP ( 'NONE', ( #5581, #20762, #10951, #12533 ) ) ;
#4653 = VERTEX_POINT ( 'NONE', #12859 ) ;
#4654 = DIRECTION ( 'NONE',  ( -0.5000000000047110094, -0.8660254037817188832, 0.000000000000000000 ) ) ;
#4655 = EDGE_CURVE ( 'NONE', #7929, #18142, #22820, .T. ) ;
#4656 = ORIENTED_EDGE ( 'NONE', *, *, #13738, .F. ) ;
#4657 = CARTESIAN_POINT ( 'NONE',  ( 9.802483769510930145, -3543.356150272095874, 2254.879165045093032 ) ) ;
#4658 = DATE_TIME_ROLE ( 'classification_date' ) ;
#4659 = CARTESIAN_POINT ( 'NONE',  ( 3.048000000000000043, -3544.061999999999898, 2239.009999999999764 ) ) ;
#4660 = DIRECTION ( 'NONE',  ( -1.000000000000000000, 0.000000000000000000, 0.000000000000000000 ) ) ;
#4661 = CYLINDRICAL_SURFACE ( 'NONE', #20078, 0.3809999999998115450 ) ;
#4662 = CIRCLE ( 'NONE', #10655, 5.460999999999938126 ) ;
#4663 = CARTESIAN_POINT ( 'NONE',  ( 12.69999999999999929, -3599.497499999999945, 2290.241799999999785 ) ) ;
#4664 = AXIS2_PLACEMENT_3D ( 'NONE', #7673, #18566, #16801 ) ;
#4665 = CYLINDRICAL_SURFACE ( 'NONE', #12856, 0.7619999999999294005 ) ;
#4666 = AXIS2_PLACEMENT_3D ( 'NONE', #16216, #12929, #11177 ) ;
#4667 = DIRECTION ( 'NONE',  ( 0.000000000000000000, 0.000000000000000000, -1.000000000000000000 ) ) ;
#4668 = ORIENTED_EDGE ( 'NONE', *, *, #15590, .F. ) ;
#4669 = DIRECTION ( 'NONE',  ( 0.000000000000000000, 1.000000000000000000, 0.000000000000000000 ) ) ;
#4670 = ADVANCED_FACE ( 'NONE', ( #3832 ), #20018, .T. ) ;
#4671 = DIRECTION ( 'NONE',  ( 0.8660254037827048723, 0.5000000000030029312, 0.000000000000000000 ) ) ;
#4672 = ORIENTED_EDGE ( 'NONE', *, *, #20736, .F. ) ;
#4673 = CARTESIAN_POINT ( 'NONE',  ( 10.36831320285999958, -3578.148799999999937, 2242.820000000000164 ) ) ;
#4674 = CARTESIAN_POINT ( 'NONE',  ( 147.3199999999999932, -3694.509865589844594, 2260.599999999999454 ) ) ;
#4675 = EDGE_CURVE ( 'NONE', #1205, #2446, #10112, .T. ) ;
#4676 = EDGE_LOOP ( 'NONE', ( #1747, #16232, #4198, #18671 ) ) ;
#4677 = EDGE_CURVE ( 'NONE', #22087, #14878, #8246, .T. ) ;
#4678 = ORIENTED_EDGE ( 'NONE', *, *, #16727, .F. ) ;
#4679 = DIRECTION ( 'NONE',  ( 0.000000000000000000, 0.000000000000000000, -1.000000000000000000 ) ) ;
#4680 = CIRCLE ( 'NONE', #1314, 3.606799999999993567 ) ;
#4681 = CIRCLE ( 'NONE', #12935, 1.269999999999882334 ) ;
#4682 = EDGE_LOOP ( 'NONE', ( #6133, #20929, #18050 ) ) ;
#4683 = VECTOR ( 'NONE', #3149, 1000.000000000000227 ) ;
#4684 = LINE ( 'NONE', #11835, #10327 ) ;
#4685 = DIRECTION ( 'NONE',  ( 0.000000000000000000, 0.000000000000000000, -1.000000000000000000 ) ) ;
#4686 = DIRECTION ( 'NONE',  ( 1.000000000000000000, 0.000000000000000000, 0.000000000000000000 ) ) ;
#4687 = TOROIDAL_SURFACE ( 'NONE', #12555, 3.606799999999999784, 0.7620000000000000107 ) ;
#4688 = CARTESIAN_POINT ( 'NONE',  ( 141.5487975361088218, -3581.657297964314694, 2247.911507805317342 ) ) ;
#4689 = VERTEX_POINT ( 'NONE', #14514 ) ;
#4690 = CARTESIAN_POINT ( 'NONE',  ( 138.7771837643548452, -3582.192323009303436, 2257.629692224586051 ) ) ;
#4691 = APPROVAL_DATE_TIME ( #22729, #12204 ) ;
#4692 = LINE ( 'NONE', #8333, #10379 ) ;
#4693 = CARTESIAN_POINT ( 'NONE',  ( 20.63610976348933690, -3543.391099285847304, 2259.808358094443065 ) ) ;
#4694 = ADVANCED_FACE ( 'NONE', ( #7364 ), #16713, .F. ) ;
#4695 = CARTESIAN_POINT ( 'NONE',  ( 134.1088469025876861, -3658.321902597664575, 2245.203711442572057 ) ) ;
#4696 = B_SPLINE_CURVE_WITH_KNOTS ( 'NONE', 3,
 ( #8525, #23030, #6657, #10619, #5354, #17526, #19062, #15782, #19300, #3003, #13908, #13793, #1473, #20938, #12030, #10265, #1360, #15668, #5004, #3584, #3697, #7675, #10851, #16578, #423, #12956, #21748, #1947, #18339, #12494, #2295 ),
 .UNSPECIFIED., .F., .F.,
 ( 4, 2, 2, 2, 2, 2, 1, 2, 2, 2, 2, 1, 1, 2, 2, 2, 4 ),
 ( 0.000000000000000000, 0.1250000000025272839, 0.1875000000034570125, 0.2500000000043867687, 0.3750000000065028538, 0.4375000000078326234, 0.4687500000080585538, 0.4843750000083739127, 0.5000000000086892715, 0.6250000000084229290, 0.6875000000085297325, 0.7187500000089692698, 0.7343750000091889829, 0.7421875000094193542, 0.7500000000096496144, 0.8750000000048248072, 1.000000000000000000 ),
 .UNSPECIFIED. ) ;
#4697 = AXIS2_PLACEMENT_3D ( 'NONE', #8811, #23085, #20146 ) ;
#4698 = ORIENTED_EDGE ( 'NONE', *, *, #8999, .F. ) ;
#4699 = VECTOR ( 'NONE', #21407, 1000.000000000000000 ) ;
#4700 = DIRECTION ( 'NONE',  ( 0.000000000000000000, -1.000000000000000000, 0.000000000000000000 ) ) ;
#4701 = CIRCLE ( 'NONE', #20428, 5.460999999999938126 ) ;
#4702 = AXIS2_PLACEMENT_3D ( 'NONE', #1977, #5505, #19791 ) ;
#4703 = VERTEX_POINT ( 'NONE', #20238 ) ;
#4704 = DIRECTION ( 'NONE',  ( -1.000000000000000000, 0.000000000000000000, 0.000000000000000000 ) ) ;
#4705 =( BOUNDED_CURVE ( )  B_SPLINE_CURVE ( 3, ( #5482, #12622, #9105, #16245 ),
 .UNSPECIFIED., .F., .T. ) 
 B_SPLINE_CURVE_WITH_KNOTS ( ( 4, 4 ),
 ( 1.570796327116351643, 3.141592653589766471 ),
 .UNSPECIFIED. ) 
 CURVE ( )  GEOMETRIC_REPRESENTATION_ITEM ( )  RATIONAL_B_SPLINE_CURVE ( ( 1.000000000000000000, 0.8047378542001389912, 0.8047378542001389912, 1.000000000000000000 ) ) 
 REPRESENTATION_ITEM ( '' )  );
#4706 = EDGE_CURVE ( 'NONE', #15456, #18476, #18472, .T. ) ;
#4707 = CARTESIAN_POINT ( 'NONE',  ( 88.90000000000000568, -3644.899999999999636, 2239.009999999999764 ) ) ;
#4708 = ORIENTED_EDGE ( 'NONE', *, *, #11776, .T. ) ;
#4709 = AXIS2_PLACEMENT_3D ( 'NONE', #19019, #2845, #17599 ) ;
#4710 = DIRECTION ( 'NONE',  ( -3.322863369922961486E-14, -0.5000000000038942183, -0.8660254037821902839 ) ) ;
#4711 = DIRECTION ( 'NONE',  ( -1.000000000000000000, 0.000000000000000000, 2.324635735433000053E-14 ) ) ;
#4712 = VERTEX_POINT ( 'NONE', #7815 ) ;
#4713 = CARTESIAN_POINT ( 'NONE',  ( 10.21049783570185099, -3658.067685255140532, 2239.010000000115724 ) ) ;
#4714 = DIRECTION ( 'NONE',  ( 0.000000000000000000, 1.000000000000000000, 0.000000000000000000 ) ) ;
#4715 =( LENGTH_UNIT ( ) NAMED_UNIT ( * ) SI_UNIT ( .MILLI., .METRE. ) );
#4716 = DIRECTION ( 'NONE',  ( 0.000000000000000000, 0.000000000000000000, -1.000000000000000000 ) ) ;
#4717 = AXIS2_PLACEMENT_3D ( 'NONE', #21526, #197, #7347 ) ;
#4718 = AXIS2_PLACEMENT_3D ( 'NONE', #2971, #10118, #17263 ) ;
#4719 = LINE ( 'NONE', #8819, #1765 ) ;
#4720 = COORDINATED_UNIVERSAL_TIME_OFFSET ( 0, 0, .AHEAD. ) ;
#4721 = AXIS2_PLACEMENT_3D ( 'NONE', #4476, #11617, #20641 ) ;
#4722 = CARTESIAN_POINT ( 'NONE',  ( 12.70000000000000107, -3668.712499999999636, 2279.817639999999756 ) ) ;
#4723 = DIRECTION ( 'NONE',  ( 1.000000000000000000, 0.000000000000000000, 3.996303350731721563E-14 ) ) ;
#4724 = DIRECTION ( 'NONE',  ( -1.000000000000000000, 0.000000000000000000, 0.000000000000000000 ) ) ;
#4725 = AXIS2_PLACEMENT_3D ( 'NONE', #1586, #21168, #1466 ) ;
#4726 = EDGE_CURVE ( 'NONE', #2597, #19144, #2313, .T. ) ;
#4727 = CARTESIAN_POINT ( 'NONE',  ( 142.2098376044692714, -3658.165498732453216, 2249.440698602000793 ) ) ;
#4728 = CARTESIAN_POINT ( 'NONE',  ( 18.41499991942999870, -3579.495498070999474, 2244.618783703000190 ) ) ;
#4729 = AXIS2_PLACEMENT_3D ( 'NONE', #13322, #17055, #2764 ) ;
#4730 = EDGE_LOOP ( 'NONE', ( #17184, #2219, #1973, #1560 ) ) ;
#4731 = DIRECTION ( 'NONE',  ( -2.324635735433000053E-14, 0.000000000000000000, -1.000000000000000000 ) ) ;
#4732 = VERTEX_POINT ( 'NONE', #2204 ) ;
#4733 = CARTESIAN_POINT ( 'NONE',  ( 4.767598319208563140, -3695.602652332028356, 2259.817658126045899 ) ) ;
#4734 = VECTOR ( 'NONE', #22632, 1000.000000000000000 ) ;
#4735 = DIRECTION ( 'NONE',  ( 0.000000000000000000, -1.000000000000000000, 0.000000000000000000 ) ) ;
#4736 = ORIENTED_EDGE ( 'NONE', *, *, #4067, .T. ) ;
#4737 = ORIENTED_EDGE ( 'NONE', *, *, #12096, .F. ) ;
#4738 = CARTESIAN_POINT ( 'NONE',  ( 0.7619999999998999796, -3695.699999999999818, 2238.248000000000047 ) ) ;
#4739 = CARTESIAN_POINT ( 'NONE',  ( -8.890000000008999592, -3581.552400000000034, 2247.392000000000280 ) ) ;
#4740 = TOROIDAL_SURFACE ( 'NONE', #7745, 3.606799999999999784, 0.7620000000000000107 ) ;
#4741 = DIRECTION ( 'NONE',  ( 0.6887494619146540265, 0.000000000000000000, -0.7249994335944508483 ) ) ;
#4742 = APPLIED_DATE_AND_TIME_ASSIGNMENT ( #17305, #15331, ( #2620 ) ) ;
#4743 = EDGE_LOOP ( 'NONE', ( #5956, #1041 ) ) ;
#4744 = DIRECTION ( 'NONE',  ( 0.000000000000000000, 0.000000000000000000, -1.000000000000000000 ) ) ;
#4745 = CARTESIAN_POINT ( 'NONE',  ( 0.7620000000000000107, -3544.061999999999898, 2275.763800000000174 ) ) ;
#4746 = CARTESIAN_POINT ( 'NONE',  ( 12.69999999999999929, -3668.712499999999636, 2268.705139999999574 ) ) ;
#4747 = CARTESIAN_POINT ( 'NONE',  ( 17.79584664100706703, -3576.912150935504087, 2245.312549109999054 ) ) ;
#4748 = CARTESIAN_POINT ( 'NONE',  ( 20.56205275154204415, -3695.513274360283958, 2259.993648869947265 ) ) ;
#4749 = ORIENTED_EDGE ( 'NONE', *, *, #16887, .F. ) ;
#4750 = DATE_AND_TIME ( #15767, #14638 ) ;
#4751 = EDGE_LOOP ( 'NONE', ( #5903, #17675, #8830, #18314 ) ) ;
#4752 = CARTESIAN_POINT ( 'NONE',  ( 139.6999999999999886, -3656.660200000000714, 2257.592639999999847 ) ) ;
#4753 = AXIS2_PLACEMENT_3D ( 'NONE', #12423, #7607, #14420 ) ;
#4754 = CARTESIAN_POINT ( 'NONE',  ( 10.90284348872566333, -3581.700236517450776, 2247.212196148407202 ) ) ;
#4755 = CIRCLE ( 'NONE', #17461, 5.080000000000000071 ) ;
#4756 = CARTESIAN_POINT ( 'NONE',  ( 64.76999999999999602, -3694.938000000000102, 2286.368300000000090 ) ) ;
#4757 = ORIENTED_EDGE ( 'NONE', *, *, #9273, .T. ) ;
#4758 = DIRECTION ( 'NONE',  ( 0.000000000000000000, 0.000000000000000000, 1.000000000000000000 ) ) ;
#4759 = AXIS2_PLACEMENT_3D ( 'NONE', #10760, #1854, #8998 ) ;
#4760 = AXIS2_PLACEMENT_3D ( 'NONE', #1408, #16991, #13480 ) ;
#4761 = CARTESIAN_POINT ( 'NONE',  ( 139.6999999999999886, -3579.494999999999891, 2270.760000000000218 ) ) ;
#4762 = FACE_OUTER_BOUND ( 'NONE', #8178, .T. ) ;
#4763 = FACE_OUTER_BOUND ( 'NONE', #18761, .T. ) ;
#4764 = CARTESIAN_POINT ( 'NONE',  ( 20.32000000000000028, -3660.140000000000327, 2247.392000000000280 ) ) ;
#4765 = DIRECTION ( 'NONE',  ( -1.000000000000000000, 5.461016542361937364E-28, 2.336881798970999789E-14 ) ) ;
#4766 = ORIENTED_EDGE ( 'NONE', *, *, #2958, .T. ) ;
#4767 = CARTESIAN_POINT ( 'NONE',  ( 19.05000000000000071, -3578.860000000000127, 2247.392000000000280 ) ) ;
#4768 = LINE ( 'NONE', #10153, #2466 ) ;
#4769 = APPLIED_DATE_AND_TIME_ASSIGNMENT ( #5072, #19600, ( #19460 ) ) ;
#4770 = EDGE_CURVE ( 'NONE', #13205, #22556, #10988, .T. ) ;
#4771 = DIRECTION ( 'NONE',  ( 0.000000000000000000, -1.000000000000000000, 0.000000000000000000 ) ) ;
#4772 = DIRECTION ( 'NONE',  ( 0.000000000000000000, 0.000000000000000000, -1.000000000000000000 ) ) ;
#4773 = DIRECTION ( 'NONE',  ( -0.8660254037825932949, 0.5000000000031962211, 0.000000000000000000 ) ) ;
#4774 = ORIENTED_EDGE ( 'NONE', *, *, #5980, .F. ) ;
#4775 = VERTEX_POINT ( 'NONE', #21876 ) ;
#4776 = CIRCLE ( 'NONE', #1394, 0.3809999999999647002 ) ;
#4777 = EDGE_CURVE ( 'NONE', #14341, #6224, #17984, .T. ) ;
#4778 = CARTESIAN_POINT ( 'NONE',  ( 114.2999999999999972, -3644.899999999999636, 2239.771999999999935 ) ) ;
#4779 = EDGE_CURVE ( 'NONE', #2492, #8893, #7883, .T. ) ;
#4780 = ORIENTED_EDGE ( 'NONE', *, *, #1169, .F. ) ;
#4781 = CARTESIAN_POINT ( 'NONE',  ( 15.07352087697999998, -3581.071667653000077, 2257.848687205999795 ) ) ;
#4782 = ITEM_DEFINED_TRANSFORMATION ( 'NONE', 'NONE', #4869,  #5611 ) ;
#4783 = EDGE_CURVE ( 'NONE', #3332, #7259, #5952, .T. ) ;
#4784 = CARTESIAN_POINT ( 'NONE',  ( -12.31899999999987294, -3654.679000000000087, 2247.392000000000280 ) ) ;
#4785 = DIRECTION ( 'NONE',  ( -1.000000000000000000, 0.000000000000000000, 0.000000000000000000 ) ) ;
#4786 = DIRECTION ( 'NONE',  ( 0.000000000000000000, 0.000000000000000000, -1.000000000000000000 ) ) ;
#4787 = CARTESIAN_POINT ( 'NONE',  ( 131.5729205195000020, -3695.699999999999818, 2259.329999999999927 ) ) ;
#4788 = DIRECTION ( 'NONE',  ( 0.000000000000000000, 0.000000000000000000, -1.000000000000000000 ) ) ;
#4789 = AXIS2_PLACEMENT_3D ( 'NONE', #8016, #8241, #11874 ) ;
#4790 = EDGE_CURVE ( 'NONE', #4467, #19050, #4881, .T. ) ;
#4791 = VERTEX_POINT ( 'NONE', #9567 ) ;
#4792 = CARTESIAN_POINT ( 'NONE',  ( -6.349999999999999645, -3543.299999999999727, 2228.849999999999909 ) ) ;
#4793 = CARTESIAN_POINT ( 'NONE',  ( 35.56000000000000227, -3544.570000000000164, 2247.392000000000280 ) ) ;
#4794 = ORIENTED_EDGE ( 'NONE', *, *, #3134, .T. ) ;
#4795 = DIRECTION ( 'NONE',  ( 0.000000000000000000, 0.000000000000000000, 1.000000000000000000 ) ) ;
#4796 = CARTESIAN_POINT ( 'NONE',  ( 10.28963435466927834, -3657.994130827179561, 2249.259658297236001 ) ) ;
#4797 = EDGE_CURVE ( 'NONE', #7082, #4608, #16849, .T. ) ;
#4798 = ORIENTED_EDGE ( 'NONE', *, *, #5704, .T. ) ;
#4799 = ORIENTED_EDGE ( 'NONE', *, *, #23021, .T. ) ;
#4800 = DIRECTION ( 'NONE',  ( 0.000000000000000000, 0.000000000000000000, 1.000000000000000000 ) ) ;
#4801 = ORIENTED_EDGE ( 'NONE', *, *, #19684, .T. ) ;
#4802 = DIRECTION ( 'NONE',  ( 0.000000000000000000, -1.000000000000000000, 0.000000000000000000 ) ) ;
#4803 = DIRECTION ( 'NONE',  ( 1.000000000000000000, 0.000000000000000000, 0.000000000000000000 ) ) ;
#4804 = FACE_OUTER_BOUND ( 'NONE', #20439, .T. ) ;
#4805 = EDGE_LOOP ( 'NONE', ( #17235, #2738 ) ) ;
#4806 = CARTESIAN_POINT ( 'NONE',  ( 131.8914011584156469, -3695.418298523433350, 2260.127650043255471 ) ) ;
#4807 = COORDINATED_UNIVERSAL_TIME_OFFSET ( 0, 0, .AHEAD. ) ;
#4808 = ADVANCED_FACE ( 'NONE', ( #12744 ), #19900, .F. ) ;
#4809 = CARTESIAN_POINT ( 'NONE',  ( -6.731000000000118888, -3578.860000000000127, 2242.311999999999898 ) ) ;
#4810 = CARTESIAN_POINT ( 'NONE',  ( 151.4000000000000057, -3695.670967364599164, 2259.329999999999927 ) ) ;
#4811 = CARTESIAN_POINT ( 'NONE',  ( 59.89320000000000022, -3594.099999999999909, 2259.837999999999738 ) ) ;
#4812 = ORIENTED_EDGE ( 'NONE', *, *, #22824, .F. ) ;
#4813 = LINE ( 'NONE', #8800, #3588 ) ;
#4814 = CARTESIAN_POINT ( 'NONE',  ( -6.349999999999999645, -3694.938000000000102, 2253.487999999999829 ) ) ;
#4815 = EDGE_LOOP ( 'NONE', ( #2450, #16060, #21882, #9635 ) ) ;
#4816 = AXIS2_PLACEMENT_3D ( 'NONE', #22570, #17181, #11918 ) ;
#4817 = DIRECTION ( 'NONE',  ( -2.626182175045999872E-12, 1.000000000000000000, 0.000000000000000000 ) ) ;
#4818 = CARTESIAN_POINT ( 'NONE',  ( 12.69999999999999929, -3659.504999999999654, 2239.771999999999935 ) ) ;
#4819 = EDGE_LOOP ( 'NONE', ( #11129, #7442 ) ) ;
#4820 = ORIENTED_EDGE ( 'NONE', *, *, #8642, .T. ) ;
#4821 = CARTESIAN_POINT ( 'NONE',  ( 20.59150420445999785, -3544.527728344000025, 2260.600000000000364 ) ) ;
#4822 = DIRECTION ( 'NONE',  ( 1.000000000000000000, 0.000000000000000000, 0.000000000000000000 ) ) ;
#4823 = ORIENTED_EDGE ( 'NONE', *, *, #2098, .F. ) ;
#4824 = LINE ( 'NONE', #14093, #10208 ) ;
#4825 = LINE ( 'NONE', #22630, #11449 ) ;
#4826 = CARTESIAN_POINT ( 'NONE',  ( 12.69997737250858982, -3642.347301253999831, 2279.817639304488239 ) ) ;
#4827 = CARTESIAN_POINT ( 'NONE',  ( 53.64479999999999649, -3568.700000000000273, 2261.869999999999891 ) ) ;
#4828 = CALENDAR_DATE ( 2026, 26, 10 ) ;
#4829 = CIRCLE ( 'NONE', #8959, 1.904999999999823501 ) ;
#4830 = DIRECTION ( 'NONE',  ( -0.000000000000000000, -1.000000000000000000, -0.000000000000000000 ) ) ;
#4831 = CARTESIAN_POINT ( 'NONE',  ( 21.79320000000099711, -3670.300000000000182, 2259.837999999999738 ) ) ;
#4832 = FACE_OUTER_BOUND ( 'NONE', #2346, .T. ) ;
#4833 = AXIS2_PLACEMENT_3D ( 'NONE', #6054, #18345, #20343 ) ;
#4834 = EDGE_CURVE ( 'NONE', #9191, #7405, #3959, .T. ) ;
#4835 = CARTESIAN_POINT ( 'NONE',  ( 141.6735277291679154, -3657.455622841492641, 2248.335144904084700 ) ) ;
#4836 = ADVANCED_FACE ( 'NONE', ( #10140, #1000, #4632 ), #22672, .F. ) ;
#4837 = EDGE_CURVE ( 'NONE', #10412, #2777, #12019, .T. ) ;
#4838 = ORIENTED_EDGE ( 'NONE', *, *, #17606, .T. ) ;
#4839 = CARTESIAN_POINT ( 'NONE',  ( 136.8553092860665856, -3543.405519448711857, 2255.010836426657079 ) ) ;
#4840 = EDGE_CURVE ( 'NONE', #21716, #14725, #15327, .T. ) ;
#4841 = ORIENTED_EDGE ( 'NONE', *, *, #8064, .F. ) ;
#4842 = DIRECTION ( 'NONE',  ( 0.000000000000000000, 0.000000000000000000, -1.000000000000000000 ) ) ;
#4843 = AXIS2_PLACEMENT_3D ( 'NONE', #10284, #10167, #11572 ) ;
#4844 = CARTESIAN_POINT ( 'NONE',  ( 12.69999999999999929, -3585.971999999999753, 2274.293139999999767 ) ) ;
#4845 = ORIENTED_EDGE ( 'NONE', *, *, #8095, .T. ) ;
#4846 = ORIENTED_EDGE ( 'NONE', *, *, #4223, .T. ) ;
#4847 = APPLIED_SECURITY_CLASSIFICATION_ASSIGNMENT ( #3363, ( #10100 ) ) ;
#4848 = CARTESIAN_POINT ( 'NONE',  ( 4.707879222708684530, -3543.344914980570593, 2259.667286593787139 ) ) ;
#4849 = DIRECTION ( 'NONE',  ( -1.000000000000000000, 0.000000000000000000, 0.000000000000000000 ) ) ;
#4850 = CIRCLE ( 'NONE', #8592, 2.844800000000091700 ) ;
#4851 = CARTESIAN_POINT ( 'NONE',  ( 131.7757523116999891, -3694.430000000000291, 2260.600000000000364 ) ) ;
#4852 = EDGE_CURVE ( 'NONE', #15774, #1541, #1089, .T. ) ;
#4853 = ORIENTED_EDGE ( 'NONE', *, *, #12280, .T. ) ;
#4854 = CARTESIAN_POINT ( 'NONE',  ( -5.588000000000000078, -3543.299999999999727, 2253.487999999999829 ) ) ;
#4855 = EDGE_CURVE ( 'NONE', #18606, #18582, #8163, .T. ) ;
#4856 = CARTESIAN_POINT ( 'NONE',  ( 95.25000000000031264, -3568.700000000000273, 2250.236800000000130 ) ) ;
#4857 = DIRECTION ( 'NONE',  ( -1.206643234470999950E-12, 1.000000000000000000, 0.000000000000000000 ) ) ;
#4858 = CARTESIAN_POINT ( 'NONE',  ( 151.4000000000000057, -3695.699999999999818, 2260.570967364599255 ) ) ;
#4859 = CARTESIAN_POINT ( 'NONE',  ( 142.5448000000000093, -3659.504999999999654, 2256.063560000000052 ) ) ;
#4860 = ORIENTED_EDGE ( 'NONE', *, *, #1417, .T. ) ;
#4861 = PERSON_AND_ORGANIZATION ( #5446, #1895 ) ;
#4862 = EDGE_LOOP ( 'NONE', ( #18399, #12578, #4030, #1155, #21148, #8173 ) ) ;
#4863 = DIRECTION ( 'NONE',  ( 1.000000000000000000, 0.000000000000000000, 0.000000000000000000 ) ) ;
#4864 = ORIENTED_EDGE ( 'NONE', *, *, #11251, .F. ) ;
#4865 = DIRECTION ( 'NONE',  ( 1.000000000000000000, 0.000000000000000000, 0.000000000000000000 ) ) ;
#4866 = ORIENTED_EDGE ( 'NONE', *, *, #774, .T. ) ;
#4867 = DIRECTION ( 'NONE',  ( 3.410299865766000309E-12, -1.000000000000000000, -9.896505939573000930E-13 ) ) ;
#4868 = APPROVAL_PERSON_ORGANIZATION ( #10103, #22502, #9869 ) ;
#4869 = AXIS2_PLACEMENT_3D ( 'NONE', #11837, #6695, #815 ) ;
#4870 = EDGE_LOOP ( 'NONE', ( #20910, #15089, #3153, #11415, #14519, #7147 ) ) ;
#4871 = DIRECTION ( 'NONE',  ( 0.000000000000000000, 0.000000000000000000, -1.000000000000000000 ) ) ;
#4872 = CIRCLE ( 'NONE', #10496, 11.11250000000000071 ) ;
#4873 = FACE_OUTER_BOUND ( 'NONE', #17189, .T. ) ;
#4874 = CARTESIAN_POINT ( 'NONE',  ( 144.9127847416437191, -3661.847664638717106, 2245.116748441303116 ) ) ;
#4875 = DIRECTION ( 'NONE',  ( 0.000000000000000000, 0.000000000000000000, 1.000000000000000000 ) ) ;
#4876 = CARTESIAN_POINT ( 'NONE',  ( 11.92076576356236295, -3662.241062566742585, 2249.309941814265585 ) ) ;
#4877 = LINE ( 'NONE', #15899, #10696 ) ;
#4878 = EDGE_LOOP ( 'NONE', ( #18927, #13957 ) ) ;
#4879 = CARTESIAN_POINT ( 'NONE',  ( 136.9873132030508600, -3577.928829547506666, 2239.009999999999764 ) ) ;
#4880 = DIRECTION ( 'NONE',  ( -0.000000000000000000, 0.8660254037825932949, 0.5000000000031962211 ) ) ;
#4881 = CIRCLE ( 'NONE', #10877, 0.3809999999999647002 ) ;
#4882 = CARTESIAN_POINT ( 'NONE',  ( 55.57575231171000496, -3544.061999999999898, 2275.763800000000174 ) ) ;
#4883 = LINE ( 'NONE', #17411, #16568 ) ;
#4884 = CARTESIAN_POINT ( 'NONE',  ( 116.8400000000000034, -3544.570000000000164, 2250.236800000000130 ) ) ;
#4885 = APPROVAL_PERSON_ORGANIZATION ( #19570, #5631, #5045 ) ;
#4886 = ORIENTED_EDGE ( 'NONE', *, *, #404, .F. ) ;
#4887 =( GEOMETRIC_REPRESENTATION_CONTEXT ( 3 ) GLOBAL_UNCERTAINTY_ASSIGNED_CONTEXT ( ( #7601 ) ) GLOBAL_UNIT_ASSIGNED_CONTEXT ( ( #22486, #7982, #16872 ) ) REPRESENTATION_CONTEXT ( 'NONE', 'WORKASPACE' ) );
#4888 = ORIENTED_EDGE ( 'NONE', *, *, #18548, .T. ) ;
#4889 = ORIENTED_EDGE ( 'NONE', *, *, #13444, .F. ) ;
#4890 = CARTESIAN_POINT ( 'NONE',  ( 7.238999999999998991, -3599.497499999999945, 2290.622800000000552 ) ) ;
#4891 = EDGE_LOOP ( 'NONE', ( #9834, #5824, #9607, #3434 ) ) ;
#4892 = ADVANCED_BREP_SHAPE_REPRESENTATION ( '', ( #13798, #5611 ), #16462 ) ;
#4893 = CARTESIAN_POINT ( 'NONE',  ( 142.2556445798637412, -3658.241573636372777, 2257.890254707658642 ) ) ;
#4894 = CALENDAR_DATE ( 2026, 26, 10 ) ;
#4895 = CIRCLE ( 'NONE', #10518, 2.844800000000001550 ) ;
#4896 = LINE ( 'NONE', #17778, #21430 ) ;
#4897 = DIRECTION ( 'NONE',  ( 0.000000000000000000, 0.000000000000000000, 1.000000000000000000 ) ) ;
#4898 = CARTESIAN_POINT ( 'NONE',  ( 10.32639513556999944, -3661.081539619000068, 2257.848705702999723 ) ) ;
#4899 = DIRECTION ( 'NONE',  ( 0.000000000000000000, 0.000000000000000000, -1.000000000000000000 ) ) ;
#4900 = APPLIED_PERSON_AND_ORGANIZATION_ASSIGNMENT ( #16283, #12766, ( #13118 ) ) ;
#4901 = CARTESIAN_POINT ( 'NONE',  ( -6.730999999999999872, -3578.860000000000127, 2247.392000000000280 ) ) ;
#4902 = APPLIED_SECURITY_CLASSIFICATION_ASSIGNMENT ( #10136, ( #23174 ) ) ;
#4903 = FACE_OUTER_BOUND ( 'NONE', #8047, .T. ) ;
#4904 = VERTEX_POINT ( 'NONE', #7927 ) ;
#4905 = LOCAL_TIME ( 17, 37, 43.00000000000000000, #15880 ) ;
#4906 = LINE ( 'NONE', #15693, #10700 ) ;
#4907 = ADVANCED_FACE ( 'NONE', ( #13426 ), #1848, .T. ) ;
#4908 = DIRECTION ( 'NONE',  ( 0.000000000000000000, 0.000000000000000000, -1.000000000000000000 ) ) ;
#4909 = EDGE_LOOP ( 'NONE', ( #11353, #10116, #19494, #15122 ) ) ;
#4910 = EDGE_CURVE ( 'NONE', #21090, #13352, #19056, .T. ) ;
#4911 = CARTESIAN_POINT ( 'NONE',  ( 15.41268679716529455, -3581.061170452570423, 2239.009999999999764 ) ) ;
#4912 = CARTESIAN_POINT ( 'NONE',  ( 147.3321676912462124, -3694.709202396953970, 2260.569587683029113 ) ) ;
#4913 = ADVANCED_FACE ( 'NONE', ( #13661 ), #2883, .T. ) ;
#4914 = ORIENTED_EDGE ( 'NONE', *, *, #22442, .F. ) ;
#4915 = AXIS2_PLACEMENT_3D ( 'NONE', #18542, #6364, #16782 ) ;
#4916 = ORIENTED_EDGE ( 'NONE', *, *, #21056, .T. ) ;
#4917 = DIRECTION ( 'NONE',  ( 0.000000000000000000, 0.000000000000000000, -1.000000000000000000 ) ) ;
#4918 = ORIENTED_EDGE ( 'NONE', *, *, #6805, .F. ) ;
#4919 = CARTESIAN_POINT ( 'NONE',  ( 18.16100000000000136, -3599.497499999999945, 2296.210799999999836 ) ) ;
#4920 = APPROVAL_DATE_TIME ( #5720, #15092 ) ;
#4921 = DIRECTION ( 'NONE',  ( -2.848935406719999894E-12, 1.000000000000000000, 2.336881798978000141E-14 ) ) ;
#4922 = VERTEX_POINT ( 'NONE', #4756 ) ;
#4923 = CYLINDRICAL_SURFACE ( 'NONE', #20127, 0.7619999999998802176 ) ;
#4924 = PERSON_AND_ORGANIZATION ( #5446, #1895 ) ;
#4925 = CARTESIAN_POINT ( 'NONE',  ( 9.987313202835000681, -3597.931329546999677, 2296.591799999999694 ) ) ;
#4926 = CARTESIAN_POINT ( 'NONE',  ( 14.94291645695195925, -3581.245342914359753, 2248.943312577677716 ) ) ;
#4927 = AXIS2_PLACEMENT_3D ( 'NONE', #19255, #17360, #15500 ) ;
#4928 = CARTESIAN_POINT ( 'NONE',  ( 134.0255062626791869, -3658.825944694054215, 2244.868864689911788 ) ) ;
#4929 = VECTOR ( 'NONE', #4710, 1000.000000000000000 ) ;
#4930 = FACE_OUTER_BOUND ( 'NONE', #5659, .T. ) ;
#4931 = ORIENTED_EDGE ( 'NONE', *, *, #4371, .T. ) ;
#4932 = CARTESIAN_POINT ( 'NONE',  ( 12.69999999999999929, -3579.494999999999891, 2245.359999999999673 ) ) ;
#4933 = EDGE_CURVE ( 'NONE', #4608, #12839, #14213, .T. ) ;
#4934 = LINE ( 'NONE', #2291, #5058 ) ;
#4935 = ORIENTED_EDGE ( 'NONE', *, *, #4797, .T. ) ;
#4936 = DIRECTION ( 'NONE',  ( 0.000000000000000000, -1.000000000000000000, 0.000000000000000000 ) ) ;
#4937 = EDGE_CURVE ( 'NONE', #22994, #12111, #7751, .T. ) ;
#4938 = EDGE_CURVE ( 'NONE', #19085, #4104, #20808, .T. ) ;
#4939 = CARTESIAN_POINT ( 'NONE',  ( 64.76999999999999602, -3568.700000000000273, 2292.057900000000245 ) ) ;
#4940 = VERTEX_POINT ( 'NONE', #22206 ) ;
#4941 = FACE_OUTER_BOUND ( 'NONE', #23065, .T. ) ;
#4942 = CIRCLE ( 'NONE', #19924, 0.7619999999999294005 ) ;
#4943 = CARTESIAN_POINT ( 'NONE',  ( 133.9850000806000310, -3659.610054942478655, 2244.594903130879629 ) ) ;
#4944 = AXIS2_PLACEMENT_3D ( 'NONE', #14913, #1023, #13573 ) ;
#4945 = VERTEX_POINT ( 'NONE', #20564 ) ;
#4946 = CIRCLE ( 'NONE', #16176, 2.844800000000001550 ) ;
#4947 = CARTESIAN_POINT ( 'NONE',  ( 0.000000000000000000, -3578.860000000000127, 2250.998800000000301 ) ) ;
#4948 = CARTESIAN_POINT ( 'NONE',  ( 15.47291618100999955, -3660.140271294999820, 2250.236802488000194 ) ) ;
#4949 = FACE_OUTER_BOUND ( 'NONE', #11379, .T. ) ;
#4950 = CARTESIAN_POINT ( 'NONE',  ( 22.54063073453000143, -3694.938000000000102, 2275.763800000000174 ) ) ;
#4951 = DATE_TIME_ROLE ( 'creation_date' ) ;
#4952 = CARTESIAN_POINT ( 'NONE',  ( 9.855390812759999619, -3579.528596999999991, 2250.157115725000040 ) ) ;
#4953 = DIRECTION ( 'NONE',  ( -1.000000000000000000, 0.000000000000000000, 0.000000000000000000 ) ) ;
#4954 = DIRECTION ( 'NONE',  ( 0.000000000000000000, 0.000000000000000000, -1.000000000000000000 ) ) ;
#4955 = EDGE_CURVE ( 'NONE', #20085, #10748, #11904, .T. ) ;
#4956 = CIRCLE ( 'NONE', #21789, 2.844799999999999773 ) ;
#4957 = CARTESIAN_POINT ( 'NONE',  ( 141.8180919227771994, -3657.605902934063579, 2248.684766514065359 ) ) ;
#4958 = CIRCLE ( 'NONE', #3079, 0.7619999999999294005 ) ;
#4959 = ORIENTED_EDGE ( 'NONE', *, *, #18982, .F. ) ;
#4960 = TOROIDAL_SURFACE ( 'NONE', #3841, 4.114799999999999791, 1.270000000000000018 ) ;
#4961 = CARTESIAN_POINT ( 'NONE',  ( 35.25520000000000209, -3644.899999999999636, 2259.837999999999738 ) ) ;
#4962 = AXIS2_PLACEMENT_3D ( 'NONE', #12501, #19651, #12733 ) ;
#4963 = VERTEX_POINT ( 'NONE', #19053 ) ;
#4964 = ORIENTED_EDGE ( 'NONE', *, *, #17246, .T. ) ;
#4965 = EDGE_CURVE ( 'NONE', #8583, #16226, #20928, .T. ) ;
#4966 = DIRECTION ( 'NONE',  ( 0.000000000000000000, -1.000000000000000000, 0.000000000000000000 ) ) ;
#4967 = ORIENTED_EDGE ( 'NONE', *, *, #7445, .T. ) ;
#4968 = ORIENTED_EDGE ( 'NONE', *, *, #2258, .T. ) ;
#4969 = FACE_OUTER_BOUND ( 'NONE', #20069, .T. ) ;
#4970 = DIRECTION ( 'NONE',  ( 0.7249994335944036639, 0.000000000000000000, 0.6887494619147036534 ) ) ;
#4971 = AXIS2_PLACEMENT_3D ( 'NONE', #11295, #637, #4381 ) ;
#4972 = CARTESIAN_POINT ( 'NONE',  ( 20.32000000000000028, -3670.300000000000182, 2289.213099999999940 ) ) ;
#4973 = ADVANCED_FACE ( 'NONE', ( #2538 ), #9786, .T. ) ;
#4974 = ORIENTED_EDGE ( 'NONE', *, *, #3409, .T. ) ;
#4975 = EDGE_CURVE ( 'NONE', #2462, #7518, #5231, .T. ) ;
#4976 = CARTESIAN_POINT ( 'NONE',  ( 152.4000000000000057, -3544.061999999999898, 2275.763800000000174 ) ) ;
#4977 = CARTESIAN_POINT ( 'NONE',  ( 12.70000000003999929, -3582.187399999999798, 2242.820000000000164 ) ) ;
#4978 = CARTESIAN_POINT ( 'NONE',  ( 12.69999999996000106, -3602.189899999999852, 2296.210799999999836 ) ) ;
#4979 = VECTOR ( 'NONE', #3793, 1000.000000000000000 ) ;
#4980 = DIRECTION ( 'NONE',  ( 0.000000000000000000, -1.165588477296860248E-12, 1.000000000000000000 ) ) ;
#4981 = ORIENTED_EDGE ( 'NONE', *, *, #8301, .T. ) ;
#4982 = CALENDAR_DATE ( 2026, 26, 10 ) ;
#4983 = AXIS2_PLACEMENT_3D ( 'NONE', #14956, #6166, #11097 ) ;
#4984 = EDGE_LOOP ( 'NONE', ( #3439, #3907, #19440, #13566, #2737, #13587, #4396, #10941, #11277, #7859 ) ) ;
#4985 = CARTESIAN_POINT ( 'NONE',  ( 50.79999999999999716, -3619.500000000000000, 2239.771999999999935 ) ) ;
#4986 = ORIENTED_EDGE ( 'NONE', *, *, #13454, .T. ) ;
#4987 = EDGE_CURVE ( 'NONE', #10571, #473, #17186, .T. ) ;
#4988 =( BOUNDED_CURVE ( )  B_SPLINE_CURVE ( 3, ( #11704, #18862, #4343, #2803 ),
 .UNSPECIFIED., .F., .T. ) 
 B_SPLINE_CURVE_WITH_KNOTS ( ( 4, 4 ),
 ( 4.051959034059917173E-16, 1.570796326496385786 ),
 .UNSPECIFIED. ) 
 CURVE ( )  GEOMETRIC_REPRESENTATION_ITEM ( )  RATIONAL_B_SPLINE_CURVE ( ( 1.000000000000000000, 0.8047378541947246555, 0.8047378541947246555, 1.000000000000000000 ) ) 
 REPRESENTATION_ITEM ( '' )  );
#4989 = CARTESIAN_POINT ( 'NONE',  ( 10.31443137789909237, -3581.044692580274841, 2249.214089242949285 ) ) ;
#4990 = ORIENTED_EDGE ( 'NONE', *, *, #18452, .T. ) ;
#4991 = DIRECTION ( 'NONE',  ( 0.000000000000000000, 0.000000000000000000, -1.000000000000000000 ) ) ;
#4992 = ORIENTED_EDGE ( 'NONE', *, *, #18653, .T. ) ;
#4993 = AXIS2_PLACEMENT_3D ( 'NONE', #3630, #1876, #1998 ) ;
#4994 = ADVANCED_FACE ( 'NONE', ( #3107 ), #10255, .T. ) ;
#4995 = FACE_BOUND ( 'NONE', #15659, .T. ) ;
#4996 = EDGE_CURVE ( 'NONE', #10545, #1677, #11566, .T. ) ;
#4997 = AXIS2_PLACEMENT_3D ( 'NONE', #9954, #4685, #20228 ) ;
#4998 = CARTESIAN_POINT ( 'NONE',  ( 20.09942059832000183, -3694.430000000000291, 2260.390449568000349 ) ) ;
#4999 = PLANE ( 'NONE',  #10724 ) ;
#5000 = TOROIDAL_SURFACE ( 'NONE', #15857, 3.606799999998999695, 0.7620000000000000107 ) ;
#5001 = DIRECTION ( 'NONE',  ( 0.000000000000000000, 0.000000000000000000, 1.000000000000000000 ) ) ;
#5002 = CARTESIAN_POINT ( 'NONE',  ( 11.29225843401678198, -3661.977178471061961, 2249.564116967847440 ) ) ;
#5003 = CLOSED_SHELL ( 'NONE', ( #12373, #21420, #19860, #4913, #3679, #18468, #5593, #15454, #21466, #20327, #21249, #913, #11676, #19978, #9153, #22176, #11266, #16929, #18419, #11961, #1114, #13604, #6350, #9646, #20187, #19755 ) ) ;
#5004 = CARTESIAN_POINT ( 'NONE',  ( 147.5484590635937820, -3543.507962131723616, 2260.027583316409618 ) ) ;
#5005 = ORIENTED_EDGE ( 'NONE', *, *, #16424, .F. ) ;
#5006 = CARTESIAN_POINT ( 'NONE',  ( -12.31900000000000084, -3577.513799999878302, 2245.060313203211081 ) ) ;
#5007 = CARTESIAN_POINT ( 'NONE',  ( -5.588000000000000078, -3544.061999999999898, 2253.487999999999829 ) ) ;
#5008 = EDGE_CURVE ( 'NONE', #21028, #15441, #4829, .T. ) ;
#5009 = LINE ( 'NONE', #22915, #21662 ) ;
#5010 = CARTESIAN_POINT ( 'NONE',  ( 14.95049008878873131, -3657.764820619780494, 2248.957728567762842 ) ) ;
#5011 = LINE ( 'NONE', #12153, #12811 ) ;
#5012 = EDGE_LOOP ( 'NONE', ( #22238, #17207, #17566, #4310 ) ) ;
#5013 = CIRCLE ( 'NONE', #15850, 3.606799999999993567 ) ;
#5014 = ORIENTED_EDGE ( 'NONE', *, *, #13406, .F. ) ;
#5015 = EDGE_LOOP ( 'NONE', ( #8119, #1278, #899, #5458 ) ) ;
#5016 = DIRECTION ( 'NONE',  ( -0.8660254037827048723, 0.5000000000030029312, 0.000000000000000000 ) ) ;
#5017 = ORIENTED_EDGE ( 'NONE', *, *, #2428, .T. ) ;
#5018 = CARTESIAN_POINT ( 'NONE',  ( 142.3985385404256760, -3658.585513653864382, 2257.925021593836391 ) ) ;
#5019 = APPROVAL_DATE_TIME ( #8541, #1885 ) ;
#5020 = CARTESIAN_POINT ( 'NONE',  ( 0.7620000000000000107, -3544.061999999999898, 2296.591799999999694 ) ) ;
#5021 = CARTESIAN_POINT ( 'NONE',  ( 9.855200508358999301, -3659.504986005999854, 2257.962940201000038 ) ) ;
#5022 = CARTESIAN_POINT ( 'NONE',  ( 132.3005794017000198, -3694.430000000000291, 2260.390449568000349 ) ) ;
#5023 = ADVANCED_FACE ( 'NONE', ( #19515 ), #19288, .T. ) ;
#5024 = DIRECTION ( 'NONE',  ( -1.000000000000000000, 0.000000000000000000, 0.000000000000000000 ) ) ;
#5025 = DIRECTION ( 'NONE',  ( -1.000000000000000000, 0.000000000000000000, 2.324635735433000053E-14 ) ) ;
#5026 = DIRECTION ( 'NONE',  ( 0.000000000000000000, 0.000000000000000000, 1.000000000000000000 ) ) ;
#5027 = ORIENTED_EDGE ( 'NONE', *, *, #11548, .T. ) ;
#5028 = TOROIDAL_SURFACE ( 'NONE', #20006, 3.606799999999999784, 0.7620000000000000107 ) ;
#5029 = DIRECTION ( 'NONE',  ( -0.7249994335945011414, 0.000000000000000000, -0.6887494619146010688 ) ) ;
#5030 = DIRECTION ( 'NONE',  ( 0.000000000000000000, 0.000000000000000000, 1.000000000000000000 ) ) ;
#5031 = AXIS2_PLACEMENT_3D ( 'NONE', #195, #18114, #11090 ) ;
#5032 = ORIENTED_EDGE ( 'NONE', *, *, #12878, .F. ) ;
#5033 = DIRECTION ( 'NONE',  ( 1.000000000000000000, 0.000000000000000000, 0.000000000000000000 ) ) ;
#5034 = CARTESIAN_POINT ( 'NONE',  ( 10.58528415310206938, -3657.602126776196656, 2248.677371791971382 ) ) ;
#5035 = ORIENTED_EDGE ( 'NONE', *, *, #10788, .T. ) ;
#5036 = CARTESIAN_POINT ( 'NONE',  ( 132.2269032045000188, -3694.556024844999683, 2260.454626673999883 ) ) ;
#5037 = ORIENTED_EDGE ( 'NONE', *, *, #21895, .T. ) ;
#5038 = APPLIED_DATE_AND_TIME_ASSIGNMENT ( #12855, #14511, ( #3396 ) ) ;
#5039 = DIRECTION ( 'NONE',  ( 0.000000000000000000, -1.000000000000000000, 0.000000000000000000 ) ) ;
#5040 = PERSON_AND_ORGANIZATION ( #5446, #1895 ) ;
#5041 = CARTESIAN_POINT ( 'NONE',  ( 136.8551999999999964, -3579.495007806000103, 2250.165025852999861 ) ) ;
#5042 = VERTEX_POINT ( 'NONE', #12132 ) ;
#5043 = CARTESIAN_POINT ( 'NONE',  ( 131.6470296295221090, -3695.700000000016189, 2259.515609107377259 ) ) ;
#5044 = CIRCLE ( 'NONE', #3919, 0.7619999999999987894 ) ;
#5045 = APPROVAL_ROLE ( '' ) ;
#5046 = AXIS2_PLACEMENT_3D ( 'NONE', #18, #1883, #7167 ) ;
#5047 = CIRCLE ( 'NONE', #13262, 3.606799999999993567 ) ;
#5048 = LINE ( 'NONE', #13725, #1789 ) ;
#5049 = DIRECTION ( 'NONE',  ( 0.000000000000000000, 1.000000000000000000, 0.000000000000000000 ) ) ;
#5050 = CARTESIAN_POINT ( 'NONE',  ( 134.1731578100668401, -3658.050678563296970, 2245.461022134579252 ) ) ;
#5051 = CARTESIAN_POINT ( 'NONE',  ( 0.7620000000000000107, -3544.061999999999898, 2296.591799999999694 ) ) ;
#5052 = VERTEX_POINT ( 'NONE', #22901 ) ;
#5053 = DIRECTION ( 'NONE',  ( 1.664719871139314556E-14, -1.000000000000000000, 0.000000000000000000 ) ) ;
#5054 = DIRECTION ( 'NONE',  ( 1.000000000000000000, 0.000000000000000000, 0.000000000000000000 ) ) ;
#5055 = ORIENTED_EDGE ( 'NONE', *, *, #15049, .F. ) ;
#5056 = VECTOR ( 'NONE', #21891, 1000.000000000000000 ) ;
#5057 = CARTESIAN_POINT ( 'NONE',  ( 22.54063073453000143, -3694.938000000000102, 2275.763800000000174 ) ) ;
#5058 = VECTOR ( 'NONE', #9437, 1000.000000000000000 ) ;
#5059 = CIRCLE ( 'NONE', #17386, 2.844800000000094364 ) ;
#5060 = CARTESIAN_POINT ( 'NONE',  ( 86.05520000000001346, -3594.099999999999909, 2239.771999999999935 ) ) ;
#5061 = CIRCLE ( 'NONE', #16661, 2.844800000000091700 ) ;
#5062 = ORIENTED_EDGE ( 'NONE', *, *, #19543, .T. ) ;
#5063 = ORIENTED_EDGE ( 'NONE', *, *, #15852, .F. ) ;
#5064 = FACE_OUTER_BOUND ( 'NONE', #15399, .T. ) ;
#5065 = CARTESIAN_POINT ( 'NONE',  ( 142.4126867972053674, -3661.071170452545175, 2239.009999999999764 ) ) ;
#5066 = ORIENTED_EDGE ( 'NONE', *, *, #10438, .F. ) ;
#5067 = APPLIED_PERSON_AND_ORGANIZATION_ASSIGNMENT ( #20557, #18467, ( #13121 ) ) ;
#5068 = CARTESIAN_POINT ( 'NONE',  ( 139.6999999999999886, -3659.504999999999654, 2246.630000000000109 ) ) ;
#5069 = CYLINDRICAL_SURFACE ( 'NONE', #20591, 5.715000000000999947 ) ;
#5070 = DIRECTION ( 'NONE',  ( 0.000000000000000000, 0.000000000000000000, -1.000000000000000000 ) ) ;
#5071 = FACE_OUTER_BOUND ( 'NONE', #5776, .T. ) ;
#5072 = DATE_AND_TIME ( #19721, #18334 ) ;
#5073 = EDGE_CURVE ( 'NONE', #7277, #473, #2591, .T. ) ;
#5074 = PLANE ( 'NONE',  #18946 ) ;
#5075 = CARTESIAN_POINT ( 'NONE',  ( 35.56000000000000227, -3543.300000000000182, 2243.277199999999993 ) ) ;
#5077 = ADVANCED_FACE ( 'NONE', ( #15889 ), #17875, .F. ) ;
#5076 = FACE_OUTER_BOUND ( 'NONE', #20572, .T. ) ;
#5078 = VECTOR ( 'NONE', #15724, 1000.000000000000000 ) ;
#5079 = AXIS2_PLACEMENT_3D ( 'NONE', #4077, #16608, #14865 ) ;
#5080 = PRODUCT ( 'Screw 8', 'Screw 8', '', ( #9228 ) ) ;
#5081 = EDGE_CURVE ( 'NONE', #18860, #6059, #4100, .T. ) ;
#5082 = CARTESIAN_POINT ( 'NONE',  ( 141.5504581569688298, -3657.343157095971037, 2247.943075285883879 ) ) ;
#5083 = VECTOR ( 'NONE', #16492, 1000.000000000000000 ) ;
#5084 = VERTEX_POINT ( 'NONE', #5113 ) ;
#5085 = CIRCLE ( 'NONE', #18175, 5.460999999999938126 ) ;
#5086 = DIRECTION ( 'NONE',  ( 0.000000000000000000, 0.000000000000000000, -1.000000000000000000 ) ) ;
#5087 = VERTEX_POINT ( 'NONE', #19631 ) ;
#5088 = EDGE_CURVE ( 'NONE', #12135, #18858, #20199, .T. ) ;
#5089 = ORIENTED_EDGE ( 'NONE', *, *, #15995, .T. ) ;
#5090 = VERTEX_POINT ( 'NONE', #1349 ) ;
#5091 = DIRECTION ( 'NONE',  ( -1.000000000000000000, 0.000000000000000000, 2.590196616235000036E-13 ) ) ;
#5092 = ORIENTED_EDGE ( 'NONE', *, *, #16140, .F. ) ;
#5093 = ORIENTED_EDGE ( 'NONE', *, *, #14142, .T. ) ;
#5094 = CARTESIAN_POINT ( 'NONE',  ( 4.769683475340658951, -3543.399485435076713, 2259.822725891639948 ) ) ;
#5095 = ADVANCED_FACE ( 'NONE', ( #17754 ), #12739, .T. ) ;
#5096 = AXIS2_PLACEMENT_3D ( 'NONE', #8757, #14264, #10622 ) ;
#5097 = CARTESIAN_POINT ( 'NONE',  ( 95.25000000000000000, -3694.430000000000291, 2247.392000000000280 ) ) ;
#5098 = VECTOR ( 'NONE', #22443, 1000.000000000000114 ) ;
#5099 = CARTESIAN_POINT ( 'NONE',  ( 127.0000000000000000, -3670.300000000000182, 2261.869999999999891 ) ) ;
#5100 = VERTEX_POINT ( 'NONE', #21394 ) ;
#5101 = AXIS2_PLACEMENT_3D ( 'NONE', #18043, #463, #14765 ) ;
#5102 = DIRECTION ( 'NONE',  ( 1.000000000000000000, 0.000000000000000000, 0.000000000000000000 ) ) ;
#5103 = CYLINDRICAL_SURFACE ( 'NONE', #20951, 5.460999999999938126 ) ;
#5104 = DIRECTION ( 'NONE',  ( -0.8660254037824819395, 0.5000000000033889558, 0.000000000000000000 ) ) ;
#5105 = CARTESIAN_POINT ( 'NONE',  ( 12.69999999997316742, -3596.622870510377652, 2296.591799999921477 ) ) ;
#5106 = ORIENTED_EDGE ( 'NONE', *, *, #10879, .F. ) ;
#5107 = PERSON_AND_ORGANIZATION ( #5446, #1895 ) ;
#5108 = EDGE_LOOP ( 'NONE', ( #14151, #8117 ) ) ;
#5109 = VECTOR ( 'NONE', #2581, 1000.000000000000000 ) ;
#5110 = FACE_OUTER_BOUND ( 'NONE', #4572, .T. ) ;
#5111 = EDGE_CURVE ( 'NONE', #4017, #8952, #13081, .T. ) ;
#5112 = CARTESIAN_POINT ( 'NONE',  ( 10.55027246081846215, -3581.358398341555585, 2248.752751047937636 ) ) ;
#5113 = CARTESIAN_POINT ( 'NONE',  ( 97.99320000000000164, -3670.300000000000182, 2260.600000000000364 ) ) ;
#5114 = ORIENTED_EDGE ( 'NONE', *, *, #14409, .T. ) ;
#5115 = CARTESIAN_POINT ( 'NONE',  ( 57.14999999999999858, -3670.300000000000182, 2250.236800000000130 ) ) ;
#5116 = ADVANCED_FACE ( 'NONE', ( #23132 ), #12485, .T. ) ;
#5117 = CIRCLE ( 'NONE', #20815, 0.7619999999999294005 ) ;
#5118 = EDGE_CURVE ( 'NONE', #9059, #10931, #10828, .T. ) ;
#5119 = ADVANCED_FACE ( 'NONE', ( #21512 ), #5463, .F. ) ;
#5120 = DIRECTION ( 'NONE',  ( 0.000000000000000000, 1.000000000000000000, 0.000000000000000000 ) ) ;
#5121 = CARTESIAN_POINT ( 'NONE',  ( 9.855200508393231473, -3579.494999998446929, 2257.962940200991852 ) ) ;
#5122 = CARTESIAN_POINT ( 'NONE',  ( 139.6999999999999886, -3659.504999999999654, 2270.760000000000218 ) ) ;
#5123 = AXIS2_PLACEMENT_3D ( 'NONE', #21633, #12835, #413 ) ;
#5124 = CARTESIAN_POINT ( 'NONE',  ( 10.70420337415141887, -3661.532743059901350, 2249.872907817715713 ) ) ;
#5125 = ORIENTED_EDGE ( 'NONE', *, *, #1353, .T. ) ;
#5126 = CARTESIAN_POINT ( 'NONE',  ( 142.4126867973298545, -3657.938829547075329, 2239.009999999999764 ) ) ;
#5127 = EDGE_LOOP ( 'NONE', ( #14291, #1496, #834, #1537 ) ) ;
#5128 = CARTESIAN_POINT ( 'NONE',  ( -6.730999999999999872, -3578.860000000000127, 2247.392000000000280 ) ) ;
#5129 = CARTESIAN_POINT ( 'NONE',  ( -8.890000000004999237, -3581.552400000000034, 2247.392000000000280 ) ) ;
#5130 = CYLINDRICAL_SURFACE ( 'NONE', #4816, 2.844799999999994444 ) ;
#5131 = CARTESIAN_POINT ( 'NONE',  ( 14.82996365613828260, -3657.619199960707647, 2248.710555545362240 ) ) ;
#5132 = CARTESIAN_POINT ( 'NONE',  ( 12.69999999999999929, -3579.494999999999891, 2245.359999999999673 ) ) ;
#5133 = CIRCLE ( 'NONE', #10407, 1.269999999999882334 ) ;
#5134 = DIRECTION ( 'NONE',  ( 0.000000000000000000, 1.000000000000000000, 0.000000000000000000 ) ) ;
#5135 = EDGE_CURVE ( 'NONE', #16093, #11557, #15699, .T. ) ;
#5136 = ORIENTED_EDGE ( 'NONE', *, *, #2768, .F. ) ;
#5137 = AXIS2_PLACEMENT_3D ( 'NONE', #16675, #18436, #20426 ) ;
#5138 = CARTESIAN_POINT ( 'NONE',  ( 110.6932000000009992, -3594.099999999999909, 2239.771999999999935 ) ) ;
#5139 = VECTOR ( 'NONE', #17197, 1000.000000000000000 ) ;
#5140 = DIRECTION ( 'NONE',  ( 0.000000000000000000, -1.000000000000000000, 0.000000000000000000 ) ) ;
#5141 = DIRECTION ( 'NONE',  ( 1.000000000000000000, 5.432398939370942693E-28, -2.324635735433000053E-14 ) ) ;
#5142 = AXIS2_PLACEMENT_3D ( 'NONE', #10847, #18107, #14718 ) ;
#5143 = DIRECTION ( 'NONE',  ( 0.000000000000000000, 0.000000000000000000, 1.000000000000000000 ) ) ;
#5144 = CARTESIAN_POINT ( 'NONE',  ( 10.18227454630999951, -3660.839269783999953, 2257.881334183000035 ) ) ;
#5145 = CARTESIAN_POINT ( 'NONE',  ( 127.0000000000000000, -3619.500000000000000, 2259.837999999999738 ) ) ;
#5146 = EDGE_CURVE ( 'NONE', #10072, #22625, #16130, .T. ) ;
#5147 = DIRECTION ( 'NONE',  ( 0.000000000000000000, -1.000000000000000000, 0.000000000000000000 ) ) ;
#5148 = EDGE_CURVE ( 'NONE', #20964, #7890, #2181, .T. ) ;
#5149 = EDGE_CURVE ( 'NONE', #10742, #5531, #12716, .T. ) ;
#5150 = CARTESIAN_POINT ( 'NONE',  ( 18.41499999999999915, -3639.502500000000055, 2288.971800000000258 ) ) ;
#5151 = ORIENTED_EDGE ( 'NONE', *, *, #15590, .T. ) ;
#5152 = DIRECTION ( 'NONE',  ( 0.000000000000000000, 0.000000000000000000, -1.000000000000000000 ) ) ;
#5153 = CIRCLE ( 'NONE', #8140, 0.7619999999999987894 ) ;
#5154 = CARTESIAN_POINT ( 'NONE',  ( -12.70000000000008455, -3580.426170452909901, 2244.679313203224865 ) ) ;
#5155 = EDGE_LOOP ( 'NONE', ( #14576, #1623 ) ) ;
#5156 = ADVANCED_FACE ( 'NONE', ( #14936 ), #5930, .T. ) ;
#5157 = CARTESIAN_POINT ( 'NONE',  ( 4.572920519510000226, -3543.299999999999727, 2259.329999999999927 ) ) ;
#5158 = VECTOR ( 'NONE', #4577, 1000.000000000000000 ) ;
#5159 = ORIENTED_EDGE ( 'NONE', *, *, #12145, .T. ) ;
#5160 = CARTESIAN_POINT ( 'NONE',  ( 134.3755117000944210, -3581.571545880567555, 2246.524605944011000 ) ) ;
#5161 = ORIENTED_EDGE ( 'NONE', *, *, #10222, .F. ) ;
#5162 = EDGE_CURVE ( 'NONE', #553, #17865, #5175, .T. ) ;
#5163 = VERTEX_POINT ( 'NONE', #18445 ) ;
#5164 = CARTESIAN_POINT ( 'NONE',  ( 139.6999999999999886, -3659.504999999999654, 2246.630000000000109 ) ) ;
#5165 = ADVANCED_FACE ( 'NONE', ( #14711 ), #20211, .F. ) ;
#5166 = DATE_AND_TIME ( #14064, #2273 ) ;
#5167 = DIRECTION ( 'NONE',  ( -1.000000000000000000, 0.000000000000000000, 0.000000000000000000 ) ) ;
#5168 = VERTEX_POINT ( 'NONE', #9538 ) ;
#5169 = CARTESIAN_POINT ( 'NONE',  ( 20.32000000000000028, -3695.699999999999818, 2292.819899999999961 ) ) ;
#5170 = APPROVAL_ROLE ( '' ) ;
#5171 = CIRCLE ( 'NONE', #11503, 2.844800000000091700 ) ;
#5172 = DIRECTION ( 'NONE',  ( 2.803365712371000161E-12, 1.000000000000000000, 0.000000000000000000 ) ) ;
#5173 = CARTESIAN_POINT ( 'NONE',  ( 14.91976558997560431, -3581.274556505038163, 2248.897383337483916 ) ) ;
#5174 = FACE_OUTER_BOUND ( 'NONE', #14553, .T. ) ;
#5175 = CIRCLE ( 'NONE', #4045, 2.844799999998995244 ) ;
#5176 = DIRECTION ( 'NONE',  ( 2.760304743598521628E-14, 1.000000000000000000, 0.000000000000000000 ) ) ;
#5177 = DIRECTION ( 'NONE',  ( -1.000000000000000000, 0.000000000000000000, 0.000000000000000000 ) ) ;
#5178 = ORIENTED_EDGE ( 'NONE', *, *, #12435, .T. ) ;
#5179 = CARTESIAN_POINT ( 'NONE',  ( 15.40196735877819734, -3695.360820976567993, 2255.368368629970519 ) ) ;
#5180 = CARTESIAN_POINT ( 'NONE',  ( -8.890000000026999416, -3576.167599999999766, 2247.392000000000280 ) ) ;
#5181 = ORIENTED_EDGE ( 'NONE', *, *, #13966, .F. ) ;
#5182 = LINE ( 'NONE', #20882, #18461 ) ;
#5183 = AXIS2_PLACEMENT_3D ( 'NONE', #10694, #22867, #17717 ) ;
#5184 = DIRECTION ( 'NONE',  ( 1.000000000000000000, 2.331176954593497545E-12, 0.000000000000000000 ) ) ;
#5185 = EDGE_LOOP ( 'NONE', ( #3720, #8055, #19612, #11085 ) ) ;
#5186 = VERTEX_POINT ( 'NONE', #16684 ) ;
#5187 = ORIENTED_EDGE ( 'NONE', *, *, #9849, .F. ) ;
#5188 = DIRECTION ( 'NONE',  ( 0.000000000000000000, 1.000000000000000000, 0.000000000000000000 ) ) ;
#5189 = CYLINDRICAL_SURFACE ( 'NONE', #14418, 2.844800000000091700 ) ;
#5190 = ORIENTED_EDGE ( 'NONE', *, *, #10783, .T. ) ;
#5191 = FACE_OUTER_BOUND ( 'NONE', #2439, .T. ) ;
#5192 = CARTESIAN_POINT ( 'NONE',  ( 12.69999999996000106, -3642.194899999999961, 2292.781800000000203 ) ) ;
#5193 = CARTESIAN_POINT ( 'NONE',  ( 134.6199999999999761, -3659.504999999999654, 2239.009999999999764 ) ) ;
#5194 = DATE_AND_TIME ( #21477, #19834 ) ;
#5195 = CARTESIAN_POINT ( 'NONE',  ( 25.39999999999999858, -3670.300000000000182, 2239.771999999999935 ) ) ;
#5196 = DIRECTION ( 'NONE',  ( 0.000000000000000000, 0.000000000000000000, -1.000000000000000000 ) ) ;
#5197 = FACE_OUTER_BOUND ( 'NONE', #14238, .T. ) ;
#5198 = CARTESIAN_POINT ( 'NONE',  ( 137.3031193615345558, -3657.972810158548327, 2249.234928345508706 ) ) ;
#5199 = EDGE_LOOP ( 'NONE', ( #4864, #4698, #4588, #13448 ) ) ;
#5200 = VECTOR ( 'NONE', #10827, 1000.000000000000000 ) ;
#5201 = CARTESIAN_POINT ( 'NONE',  ( 134.0203227398999957, -3578.860230781999689, 2244.548186305999934 ) ) ;
#5202 = APPLIED_PERSON_AND_ORGANIZATION_ASSIGNMENT ( #13273, #12937, ( #3469 ) ) ;
#5203 = EDGE_CURVE ( 'NONE', #8201, #19707, #20872, .T. ) ;
#5204 = ORIENTED_EDGE ( 'NONE', *, *, #351, .F. ) ;
#5205 = ORIENTED_EDGE ( 'NONE', *, *, #21004, .T. ) ;
#5206 = ORIENTED_EDGE ( 'NONE', *, *, #1663, .T. ) ;
#5207 = LINE ( 'NONE', #12113, #19703 ) ;
#5208 = EDGE_CURVE ( 'NONE', #22764, #20229, #18258, .T. ) ;
#5209 = VERTEX_POINT ( 'NONE', #3689 ) ;
#5210 = ORIENTED_EDGE ( 'NONE', *, *, #16807, .T. ) ;
#5211 = CARTESIAN_POINT ( 'NONE',  ( 5.079999999832377711, -3544.253380988285699, 2260.599999999823467 ) ) ;
#5212 = EDGE_CURVE ( 'NONE', #4163, #15095, #22067, .T. ) ;
#5213 = COORDINATED_UNIVERSAL_TIME_OFFSET ( 0, 0, .AHEAD. ) ;
#5214 = CYLINDRICAL_SURFACE ( 'NONE', #12540, 1.269999999999882334 ) ;
#5215 = CARTESIAN_POINT ( 'NONE',  ( 139.6999999999999886, -3570.287499999999909, 2257.592639999999847 ) ) ;
#5216 = EDGE_CURVE ( 'NONE', #5209, #9879, #21261, .T. ) ;
#5217 = VERTEX_POINT ( 'NONE', #21631 ) ;
#5218 = FACE_OUTER_BOUND ( 'NONE', #2151, .T. ) ;
#5219 = DIRECTION ( 'NONE',  ( 0.000000000000000000, 1.000000000000000000, 0.000000000000000000 ) ) ;
#5220 = DIRECTION ( 'NONE',  ( 0.000000000000000000, 0.000000000000000000, -1.000000000000000000 ) ) ;
#5221 = VECTOR ( 'NONE', #8501, 1000.000000000000000 ) ;
#5222 = CARTESIAN_POINT ( 'NONE',  ( 15.03168679717000167, -3660.851200000000063, 2242.820000000000164 ) ) ;
#5223 = VERTEX_POINT ( 'NONE', #2055 ) ;
#5224 = APPROVAL_STATUS ( 'not_yet_approved' ) ;
#5225 = EDGE_CURVE ( 'NONE', #13878, #18081, #9644, .T. ) ;
#5226 = CARTESIAN_POINT ( 'NONE',  ( 131.8914032746874341, -3543.581701476120543, 2260.127649197567735 ) ) ;
#5227 = CARTESIAN_POINT ( 'NONE',  ( 10.82796438153653007, -3581.637321854239872, 2248.014231754040338 ) ) ;
#5228 = DIRECTION ( 'NONE',  ( 1.000000000000000000, 0.000000000000000000, 0.000000000000000000 ) ) ;
#5229 = EDGE_CURVE ( 'NONE', #3857, #16025, #2177, .T. ) ;
#5230 = EDGE_LOOP ( 'NONE', ( #15752, #18091, #17816, #17255 ) ) ;
#5231 = CIRCLE ( 'NONE', #5608, 0.7620000000000001217 ) ;
#5232 = DIRECTION ( 'NONE',  ( 1.000000000000000000, 0.000000000000000000, 3.996303350731721563E-14 ) ) ;
#5233 = FACE_BOUND ( 'NONE', #21994, .T. ) ;
#5234 = DIRECTION ( 'NONE',  ( 0.000000000000000000, 1.000000000000000000, 0.000000000000000000 ) ) ;
#5235 = CARTESIAN_POINT ( 'NONE',  ( 10.60701338793428050, -3661.431926821307570, 2249.926631412048664 ) ) ;
#5236 = CARTESIAN_POINT ( 'NONE',  ( 88.90000000000000568, -3594.099999999999909, 2239.771999999999935 ) ) ;
#5237 = EDGE_LOOP ( 'NONE', ( #2360, #21059 ) ) ;
#5238 = SPHERICAL_SURFACE ( 'NONE', #5793, 0.7620000000000000107 ) ;
#5239 = ADVANCED_FACE ( 'NONE', ( #7899, #8018 ), #2728, .T. ) ;
#5240 = DIRECTION ( 'NONE',  ( -1.000000000000000000, 0.000000000000000000, 0.000000000000000000 ) ) ;
#5241 = EDGE_CURVE ( 'NONE', #2780, #12180, #12224, .T. ) ;
#5242 = DIRECTION ( 'NONE',  ( -1.000000000000000000, 0.000000000000000000, 0.000000000000000000 ) ) ;
#5243 = CARTESIAN_POINT ( 'NONE',  ( 15.08392934718898459, -3657.952714460870993, 2249.210978331739170 ) ) ;
#5244 = CARTESIAN_POINT ( 'NONE',  ( 137.1599999999999966, -3694.430000000000291, 2255.774000000000342 ) ) ;
#5245 = ORIENTED_EDGE ( 'NONE', *, *, #7034, .T. ) ;
#5246 = CYLINDRICAL_SURFACE ( 'NONE', #1899, 2.844800000000091700 ) ;
#5247 = ORIENTED_EDGE ( 'NONE', *, *, #4837, .F. ) ;
#5248 = CARTESIAN_POINT ( 'NONE',  ( 132.0879339926999876, -3544.241663918999620, 2260.533847755999886 ) ) ;
#5249 = APPLIED_APPROVAL_ASSIGNMENT ( #4186, ( #22639 ) ) ;
#5250 = DIRECTION ( 'NONE',  ( 0.000000000000000000, 0.000000000000000000, -1.000000000000000000 ) ) ;
#5251 = APPROVAL_ROLE ( '' ) ;
#5252 = LINE ( 'NONE', #20954, #18045 ) ;
#5253 = DIRECTION ( 'NONE',  ( 0.000000000000000000, 0.000000000000000000, -1.000000000000000000 ) ) ;
#5254 = CARTESIAN_POINT ( 'NONE',  ( 12.69999999999999929, -3659.504999999999654, 2272.030000000000200 ) ) ;
#5255 = CARTESIAN_POINT ( 'NONE',  ( -0.7620000000000000107, -3543.299999999999727, 2253.487999999999829 ) ) ;
#5256 = CARTESIAN_POINT ( 'NONE',  ( 139.6999999999999886, -3579.494999999999891, 2244.978999999999814 ) ) ;
#5257 = CYLINDRICAL_SURFACE ( 'NONE', #21121, 0.7620000000000000107 ) ;
#5258 = ORIENTED_EDGE ( 'NONE', *, *, #13572, .F. ) ;
#5259 = AXIS2_PLACEMENT_3D ( 'NONE', #22813, #10869, #5498 ) ;
#5260 = CARTESIAN_POINT ( 'NONE',  ( 151.1299999999999955, -3544.570000000000164, 2260.600000000000364 ) ) ;
#5261 = EDGE_LOOP ( 'NONE', ( #12924, #16494, #2857 ) ) ;
#5262 = SECURITY_CLASSIFICATION ( '', '', #21100 ) ;
#5263 = FACE_OUTER_BOUND ( 'NONE', #5230, .T. ) ;
#5264 = LOCAL_TIME ( 17, 37, 43.00000000000000000, #1458 ) ;
#5265 = VERTEX_POINT ( 'NONE', #11876 ) ;
#5266 = CARTESIAN_POINT ( 'NONE',  ( 35.56000000000000227, -3694.430000000000291, 2250.236800000000130 ) ) ;
#5267 = DIRECTION ( 'NONE',  ( 1.000000000000000000, 0.000000000000000000, 0.000000000000000000 ) ) ;
#5268 = ORIENTED_EDGE ( 'NONE', *, *, #8131, .T. ) ;
#5269 = EDGE_LOOP ( 'NONE', ( #568, #13962, #11749, #12698 ) ) ;
#5270 = ADVANCED_FACE ( 'NONE', ( #10432, #18558 ), #970, .F. ) ;
#5271 = EDGE_CURVE ( 'NONE', #16784, #12197, #18781, .T. ) ;
#5272 = EDGE_CURVE ( 'NONE', #1840, #6749, #22405, .T. ) ;
#5273 = CARTESIAN_POINT ( 'NONE',  ( 15.44319999999931525, -3580.373257047475363, 2255.967040000000907 ) ) ;
#5274 = ORIENTED_EDGE ( 'NONE', *, *, #620, .F. ) ;
#5275 = DIRECTION ( 'NONE',  ( 0.000000000000000000, 0.000000000000000000, -1.000000000000000000 ) ) ;
#5276 = APPROVAL_DATE_TIME ( #6811, #4186 ) ;
#5277 = APPLICATION_CONTEXT ( 'configuration controlled 3d designs of mechanical parts and assemblies' ) ;
#5278 = DIRECTION ( 'NONE',  ( 0.000000000000000000, 0.000000000000000000, -1.000000000000000000 ) ) ;
#5279 = APPLIED_APPROVAL_ASSIGNMENT ( #15483, ( #9398 ) ) ;
#5280 = CARTESIAN_POINT ( 'NONE',  ( 6.985000002048999512, -3579.494756921999851, 2244.617465693000213 ) ) ;
#5281 = ADVANCED_FACE ( 'NONE', ( #9760 ), #11522, .F. ) ;
#5282 = APPLIED_APPROVAL_ASSIGNMENT ( #12070, ( #12786 ) ) ;
#5283 = DIRECTION ( 'NONE',  ( 0.000000000000000000, 0.000000000000000000, 1.000000000000000000 ) ) ;
#5284 = CARTESIAN_POINT ( 'NONE',  ( 101.5999999999999943, -3619.500000000000000, 2239.771999999999935 ) ) ;
#5285 = DIRECTION ( 'NONE',  ( 5.432398939370942693E-28, 1.000000000000000000, 2.336881798971000105E-14 ) ) ;
#5286 = ORIENTED_EDGE ( 'NONE', *, *, #19519, .F. ) ;
#5287 = DIRECTION ( 'NONE',  ( 0.000000000000000000, -2.336881798971000105E-14, 1.000000000000000000 ) ) ;
#5288 = EDGE_CURVE ( 'NONE', #12668, #22201, #19012, .T. ) ;
#5289 = VECTOR ( 'NONE', #20912, 1000.000000000000000 ) ;
#5290 = ADVANCED_FACE ( 'NONE', ( #8243 ), #19763, .T. ) ;
#5291 = DIRECTION ( 'NONE',  ( -0.5000000000007168710, 0.8660254037840248165, 0.000000000000000000 ) ) ;
#5292 = ORIENTED_EDGE ( 'NONE', *, *, #21685, .T. ) ;
#5293 = CARTESIAN_POINT ( 'NONE',  ( 38.10000000000000142, -3594.099999999999909, 2239.771999999999935 ) ) ;
#5294 = LINE ( 'NONE', #19586, #1629 ) ;
#5295 = PLANE ( 'NONE',  #571 ) ;
#5296 = ORIENTED_EDGE ( 'NONE', *, *, #20664, .T. ) ;
#5297 = ORIENTED_EDGE ( 'NONE', *, *, #2510, .F. ) ;
#5298 = DIRECTION ( 'NONE',  ( 0.8660254037840259267, -0.5000000000007149836, 0.000000000000000000 ) ) ;
#5299 = CARTESIAN_POINT ( 'NONE',  ( 1.270000000000000018, -3695.699999999999818, 2259.329999999999927 ) ) ;
#5300 = VERTEX_POINT ( 'NONE', #11406 ) ;
#5301 = CARTESIAN_POINT ( 'NONE',  ( 20.32000000000000028, -3694.938000000000102, 2289.213099999999940 ) ) ;
#5302 = EDGE_CURVE ( 'NONE', #7171, #1092, #12279, .T. ) ;
#5303 = CARTESIAN_POINT ( 'NONE',  ( 3.048000000000000043, -3694.938000000000102, 2229.612000000000080 ) ) ;
#5304 = CARTESIAN_POINT ( 'NONE',  ( 137.9648833203323193, -3657.242990386724159, 2257.727830850464670 ) ) ;
#5306 = DIRECTION ( 'NONE',  ( -0.5000000000040877302, 0.8660254037820785955, 0.000000000000000000 ) ) ;
#5305 = CIRCLE ( 'NONE', #18392, 6.476999999999001112 ) ;
#5307 = CALENDAR_DATE ( 2026, 26, 10 ) ;
#5308 = TOROIDAL_SURFACE ( 'NONE', #15402, 1.524000000000000021, 0.7620000000000000107 ) ;
#5309 = CARTESIAN_POINT ( 'NONE',  ( 12.70000000023389042, -3642.634840905157944, 2296.591799999999694 ) ) ;
#5310 = CARTESIAN_POINT ( 'NONE',  ( 9.847653496145797547, -3695.602652332805974, 2254.991636092922818 ) ) ;
#5311 = VERTEX_POINT ( 'NONE', #11625 ) ;
#5312 = DIRECTION ( 'NONE',  ( -0.8660254037825932949, 0.5000000000031962211, 0.000000000000000000 ) ) ;
#5313 = CARTESIAN_POINT ( 'NONE',  ( 137.4007074334733716, -3657.828996996126989, 2249.052647309616987 ) ) ;
#5314 = VERTEX_POINT ( 'NONE', #4728 ) ;
#5315 = CARTESIAN_POINT ( 'NONE',  ( 64.76999999999999602, -3670.300000000000182, 2292.057900000000245 ) ) ;
#5316 = ORIENTED_EDGE ( 'NONE', *, *, #10557, .T. ) ;
#5317 = ORIENTED_EDGE ( 'NONE', *, *, #1795, .T. ) ;
#5318 = ORIENTED_EDGE ( 'NONE', *, *, #11923, .F. ) ;
#5319 = AXIS2_PLACEMENT_3D ( 'NONE', #8240, #8482, #13507 ) ;
#5320 = CIRCLE ( 'NONE', #4551, 0.3809999999999647002 ) ;
#5321 = CARTESIAN_POINT ( 'NONE',  ( 151.1299999999999955, -3660.140000000000327, 2247.392000000000280 ) ) ;
#5322 = ORIENTED_EDGE ( 'NONE', *, *, #9676, .T. ) ;
#5323 = EDGE_LOOP ( 'NONE', ( #6809, #8816, #22785, #11701 ) ) ;
#5324 = CARTESIAN_POINT ( 'NONE',  ( 4.722881977098646544, -3543.356150277230427, 2259.705006069447791 ) ) ;
#5325 = APPROVAL_ROLE ( '' ) ;
#5326 = DIRECTION ( 'NONE',  ( 0.000000000000000000, 0.000000000000000000, -1.000000000000000000 ) ) ;
#5327 = CARTESIAN_POINT ( 'NONE',  ( 12.69999999999999929, -3659.504999999999654, 2270.760000000000218 ) ) ;
#5328 = ORIENTED_EDGE ( 'NONE', *, *, #12801, .F. ) ;
#5329 = DIRECTION ( 'NONE',  ( 1.000000000000000000, 0.000000000000000000, 0.000000000000000000 ) ) ;
#5330 = FACE_BOUND ( 'NONE', #14463, .T. ) ;
#5331 = LINE ( 'NONE', #4978, #15821 ) ;
#5332 = SHAPE_REPRESENTATION ( 'Screw 8', ( #5611 ), #6759 ) ;
#5333 = DIRECTION ( 'NONE',  ( -1.990254351990999514E-12, 1.000000000000000000, -3.793660610075000646E-12 ) ) ;
#5334 = AXIS2_PLACEMENT_3D ( 'NONE', #19630, #3801, #3688 ) ;
#5335 = ORIENTED_EDGE ( 'NONE', *, *, #15682, .F. ) ;
#5336 = CALENDAR_DATE ( 2026, 26, 10 ) ;
#5337 = APPROVAL ( #11375, 'UNSPECIFIED' ) ;
#5338 = DIRECTION ( 'NONE',  ( 0.7249994335945011414, 0.000000000000000000, 0.6887494619146010688 ) ) ;
#5339 = AXIS2_PLACEMENT_3D ( 'NONE', #6547, #13919, #14162 ) ;
#5340 = AXIS2_PLACEMENT_3D ( 'NONE', #1379, #13812, #3367 ) ;
#5341 = AXIS2_PLACEMENT_3D ( 'NONE', #6664, #15675, #15908 ) ;
#5342 = DIRECTION ( 'NONE',  ( 1.000000000000000000, 0.000000000000000000, 0.000000000000000000 ) ) ;
#5343 = ADVANCED_FACE ( 'NONE', ( #15393 ), #5552, .T. ) ;
#5344 = CARTESIAN_POINT ( 'NONE',  ( 20.32000000000000028, -3695.699999999999818, 2289.213099999999940 ) ) ;
#5345 = EDGE_LOOP ( 'NONE', ( #14443, #1069, #16666, #7151 ) ) ;
#5346 = FACE_BOUND ( 'NONE', #18764, .T. ) ;
#5347 = EDGE_CURVE ( 'NONE', #7639, #22341, #7413, .T. ) ;
#5348 = CARTESIAN_POINT ( 'NONE',  ( 19.05000000000000071, -3575.684999999999945, 2247.392000000000280 ) ) ;
#5349 = CARTESIAN_POINT ( 'NONE',  ( 63.50000000000000000, -3644.899999999999636, 2239.771999999999935 ) ) ;
#5350 = DIRECTION ( 'NONE',  ( 0.000000000000000000, 0.000000000000000000, -1.000000000000000000 ) ) ;
#5351 = AXIS2_PLACEMENT_3D ( 'NONE', #14796, #16430, #610 ) ;
#5352 = CYLINDRICAL_SURFACE ( 'NONE', #11770, 3.175000000000149925 ) ;
#5353 = ORIENTED_EDGE ( 'NONE', *, *, #2987, .F. ) ;
#5354 = CARTESIAN_POINT ( 'NONE',  ( 147.3359348846743444, -3544.251379750038723, 2260.560039348503324 ) ) ;
#5355 = VERTEX_POINT ( 'NONE', #6269 ) ;
#5356 = DIRECTION ( 'NONE',  ( -3.599768650750962257E-14, -0.5000000000038942183, -0.8660254037821902839 ) ) ;
#5357 = AXIS2_PLACEMENT_3D ( 'NONE', #1574, #21156, #8734 ) ;
#5358 = CARTESIAN_POINT ( 'NONE',  ( 132.0583097651000060, -3694.797466901999996, 2260.545675974999995 ) ) ;
#5359 = AXIS2_PLACEMENT_3D ( 'NONE', #3650, #21813, #7407 ) ;
#5360 = CARTESIAN_POINT ( 'NONE',  ( 12.69999999999999929, -3583.940000000000055, 2268.705139999999574 ) ) ;
#5361 = CARTESIAN_POINT ( 'NONE',  ( 15.01743630476217284, -3657.855092720787525, 2249.086948850284443 ) ) ;
#5362 = CARTESIAN_POINT ( 'NONE',  ( 137.1478323087536637, -3694.709202396637011, 2255.743587683099577 ) ) ;
#5363 = CARTESIAN_POINT ( 'NONE',  ( 64.76999999999999602, -3695.699999999999818, 2289.213099999999940 ) ) ;
#5364 = VERTEX_POINT ( 'NONE', #6495 ) ;
#5365 = PRODUCT_DEFINITION ( 'UNKNOWN', '', #18354, #14646 ) ;
#5366 = AXIS2_PLACEMENT_3D ( 'NONE', #15878, #14009, #17509 ) ;
#5367 = DIRECTION ( 'NONE',  ( 0.000000000000000000, 1.000000000000000000, 0.000000000000000000 ) ) ;
#5368 = CARTESIAN_POINT ( 'NONE',  ( 10.36831320285999958, -3658.158799999999701, 2242.820000000000164 ) ) ;
#5370 = AXIS2_PLACEMENT_3D ( 'NONE', #11688, #11575, #6559 ) ;
#5369 = APPROVAL_ROLE ( '' ) ;
#5371 = DIRECTION ( 'NONE',  ( -1.000000000000000000, 0.000000000000000000, 0.000000000000000000 ) ) ;
#5372 = EDGE_CURVE ( 'NONE', #1484, #11029, #6381, .T. ) ;
#5373 = DIRECTION ( 'NONE',  ( 0.000000000000000000, 0.000000000000000000, 1.000000000000000000 ) ) ;
#5374 = CARTESIAN_POINT ( 'NONE',  ( 34.49320000000000164, -3644.899999999999636, 2259.837999999999738 ) ) ;
#5375 = AXIS2_PLACEMENT_3D ( 'NONE', #11511, #4375, #729 ) ;
#5376 = DIRECTION ( 'NONE',  ( -1.000000000000000000, 0.000000000000000000, 0.000000000000000000 ) ) ;
#5377 = ADVANCED_FACE ( 'NONE', ( #11748 ), #18904, .F. ) ;
#5378 = CIRCLE ( 'NONE', #12481, 2.844799999998995244 ) ;
#5379 = B_SPLINE_CURVE_WITH_KNOTS ( 'NONE', 3,
 ( #5244, #8760, #23038, #5362, #7351, #2079, #7013, #84, #9225, #14158, #318, #9110, #21301, #3473, #3821, #14503, #7236, #16365, #16248, #21646, #12386, #16021, #10625, #14382, #10975, #21414, #17771, #1727, #8877, #23147, #12625 ),
 .UNSPECIFIED., .F., .F.,
 ( 4, 2, 2, 2, 2, 2, 1, 2, 2, 2, 2, 1, 1, 2, 2, 2, 4 ),
 ( 0.000000000000000000, 0.1250000000013097856, 0.1875000000023017976, 0.2500000000032938097, 0.3750000000052778337, 0.4375000000059938166, 0.4687500000061067262, 0.4843750000063656858, 0.5000000000066245898, 0.6250000000102919895, 0.6875000000121920252, 0.7187500000131421540, 0.7343750000137396761, 0.7421875000141466838, 0.7500000000145535806, 0.8750000000072767348, 1.000000000000000000 ),
 .UNSPECIFIED. ) ;
#5380 = ORIENTED_EDGE ( 'NONE', *, *, #8124, .T. ) ;
#5381 = DIRECTION ( 'NONE',  ( 0.000000000000000000, 0.000000000000000000, 1.000000000000000000 ) ) ;
#5382 = ORIENTED_EDGE ( 'NONE', *, *, #9456, .T. ) ;
#5383 = DIRECTION ( 'NONE',  ( 1.000000000000000000, -0.000000000000000000, 1.224646799147353207E-16 ) ) ;
#5384 = CARTESIAN_POINT ( 'NONE',  ( 17.78000000000000114, -3659.504999999999654, 2245.359999999999673 ) ) ;
#5385 = VERTEX_POINT ( 'NONE', #17574 ) ;
#5386 = LINE ( 'NONE', #10646, #558 ) ;
#5387 = ADVANCED_FACE ( 'NONE', ( #8681 ), #6034, .T. ) ;
#5388 = ORIENTED_EDGE ( 'NONE', *, *, #11492, .T. ) ;
#5389 = FACE_OUTER_BOUND ( 'NONE', #6047, .T. ) ;
#5390 = DIRECTION ( 'NONE',  ( 0.000000000000000000, -1.000000000000000000, 0.000000000000000000 ) ) ;
#5391 = EDGE_CURVE ( 'NONE', #17185, #9415, #20147, .T. ) ;
#5392 = ORIENTED_EDGE ( 'NONE', *, *, #12284, .F. ) ;
#5393 = CARTESIAN_POINT ( 'NONE',  ( 137.3991818876238540, -3581.168941546183760, 2249.055578352219072 ) ) ;
#5394 = ORIENTED_EDGE ( 'NONE', *, *, #115, .F. ) ;
#5395 = CARTESIAN_POINT ( 'NONE',  ( 15.03168679716618961, -3658.158799999851908, 2239.167815367207822 ) ) ;
#5396 = APPLICATION_PROTOCOL_DEFINITION ( 'international standard', 'automotive_design', 2000, #22030 ) ;
#5397 = DIRECTION ( 'NONE',  ( 0.000000000000000000, 0.000000000000000000, -1.000000000000000000 ) ) ;
#5398 = DIRECTION ( 'NONE',  ( 0.000000000000000000, 0.000000000000000000, -1.000000000000000000 ) ) ;
#5399 = AXIS2_PLACEMENT_3D ( 'NONE', #3719, #328, #21881 ) ;
#5400 = LINE ( 'NONE', #14542, #21601 ) ;
#5401 = EDGE_CURVE ( 'NONE', #5562, #12834, #6361, .T. ) ;
#5402 = DIRECTION ( 'NONE',  ( 0.000000000000000000, 1.000000000000000000, 0.000000000000000000 ) ) ;
#5403 = DIRECTION ( 'NONE',  ( -1.000000000000000000, 0.000000000000000000, 0.000000000000000000 ) ) ;
#5404 = EDGE_LOOP ( 'NONE', ( #1442, #22657, #9218, #22162 ) ) ;
#5405 = CARTESIAN_POINT ( 'NONE',  ( 134.0238507593082034, -3578.829296296447410, 2244.547341334188332 ) ) ;
#5406 = EDGE_CURVE ( 'NONE', #13051, #22822, #10025, .T. ) ;
#5407 = EDGE_CURVE ( 'NONE', #18712, #3088, #2126, .T. ) ;
#5408 = DIRECTION ( 'NONE',  ( 0.000000000000000000, 0.000000000000000000, 1.000000000000000000 ) ) ;
#5409 = VERTEX_POINT ( 'NONE', #11013 ) ;
#5410 = DIRECTION ( 'NONE',  ( 0.000000000000000000, -0.8660254037817070039, 0.5000000000047313264 ) ) ;
#5411 = CARTESIAN_POINT ( 'NONE',  ( 136.8552000000001669, -3659.053785370567766, 2256.063560000000052 ) ) ;
#5412 = FACE_OUTER_BOUND ( 'NONE', #19210, .T. ) ;
#5413 = EDGE_LOOP ( 'NONE', ( #21957, #494, #10092, #20125 ) ) ;
#5414 = CARTESIAN_POINT ( 'NONE',  ( 139.6999999999999886, -3579.494999999999891, 2246.630000000000109 ) ) ;
#5415 = CARTESIAN_POINT ( 'NONE',  ( 12.69999999999999929, -3639.502500000000055, 2288.971800000000258 ) ) ;
#5416 = AXIS2_PLACEMENT_3D ( 'NONE', #4761, #10613, #12265 ) ;
#5417 = VERTEX_POINT ( 'NONE', #21226 ) ;
#5418 = VECTOR ( 'NONE', #2859, 1000.000000000000000 ) ;
#5419 = DIRECTION ( 'NONE',  ( 1.000000000000000000, -2.330758767201999921E-14, -2.339144844575000061E-14 ) ) ;
#5420 = PLANE ( 'NONE',  #2278 ) ;
#5421 = AXIS2_PLACEMENT_3D ( 'NONE', #8149, #22080, #6160 ) ;
#5422 = DIRECTION ( 'NONE',  ( 1.000000000000000000, 5.432398939370943590E-28, -2.324635735433000369E-14 ) ) ;
#5423 = DIRECTION ( 'NONE',  ( -2.324635735433000053E-14, 2.336881798971000105E-14, -1.000000000000000000 ) ) ;
#5424 = EDGE_CURVE ( 'NONE', #14745, #20703, #8911, .T. ) ;
#5425 = APPROVAL_DATE_TIME ( #6954, #7921 ) ;
#5426 = DIRECTION ( 'NONE',  ( 0.000000000000000000, 0.000000000000000000, 1.000000000000000000 ) ) ;
#5427 = CARTESIAN_POINT ( 'NONE',  ( 12.69999999999999929, -3590.289999999999964, 2268.705139999999574 ) ) ;
#5428 = VERTEX_POINT ( 'NONE', #7051 ) ;
#5429 = CARTESIAN_POINT ( 'NONE',  ( 18.29115343677415950, -3580.678095346448117, 2245.203709729950333 ) ) ;
#5430 = CARTESIAN_POINT ( 'NONE',  ( 137.1124960021244306, -3658.322399823277465, 2249.581012931923397 ) ) ;
#5431 = CIRCLE ( 'NONE', #11826, 5.715000000000884484 ) ;
#5432 = VERTEX_POINT ( 'NONE', #17922 ) ;
#5433 = CIRCLE ( 'NONE', #20391, 0.7619999999999987894 ) ;
#5434 = CIRCLE ( 'NONE', #12923, 1.269999999999882334 ) ;
#5435 = EDGE_CURVE ( 'NONE', #18165, #8539, #13035, .T. ) ;
#5436 = EDGE_LOOP ( 'NONE', ( #22074, #228, #4838, #17802 ) ) ;
#5437 = CIRCLE ( 'NONE', #21887, 3.606800000000000228 ) ;
#5438 = ORIENTED_EDGE ( 'NONE', *, *, #4359, .F. ) ;
#5439 = EDGE_LOOP ( 'NONE', ( #1091, #9150 ) ) ;
#5440 = DIRECTION ( 'NONE',  ( 0.000000000000000000, 0.000000000000000000, 1.000000000000000000 ) ) ;
#5441 = EDGE_LOOP ( 'NONE', ( #12405, #18082, #3119, #12208 ) ) ;
#5442 = ORIENTED_EDGE ( 'NONE', *, *, #2662, .F. ) ;
#5443 = DIRECTION ( 'NONE',  ( 0.000000000000000000, 0.000000000000000000, 1.000000000000000000 ) ) ;
#5444 = CALENDAR_DATE ( 2026, 26, 10 ) ;
#5445 = DIRECTION ( 'NONE',  ( 1.000000000000000000, 0.000000000000000000, 0.000000000000000000 ) ) ;
#5446 = PERSON ( 'UNSPECIFIED', 'UNSPECIFIED', 'UNSPECIFIED', ('UNSPECIFIED'), ('UNSPECIFIED'), ('UNSPECIFIED') ) ;
#5447 = FACE_OUTER_BOUND ( 'NONE', #5185, .T. ) ;
#5448 = VERTEX_POINT ( 'NONE', #16174 ) ;
#5449 = DIRECTION ( 'NONE',  ( -4.128125857118000170E-13, 1.295098308114999897E-13, 1.000000000000000000 ) ) ;
#5450 = DIRECTION ( 'NONE',  ( 1.000000000000000000, 0.000000000000000000, 0.000000000000000000 ) ) ;
#5451 = CARTESIAN_POINT ( 'NONE',  ( -8.890000000026999416, -3576.167599999999766, 2247.392000000000280 ) ) ;
#5452 = AXIS2_PLACEMENT_3D ( 'NONE', #4818, #15372, #15614 ) ;
#5453 = VECTOR ( 'NONE', #446, 1000.000000000000000 ) ;
#5454 = DIRECTION ( 'NONE',  ( 2.336881798971000105E-14, 2.336881798971000105E-14, 1.000000000000000000 ) ) ;
#5455 = EDGE_CURVE ( 'NONE', #7940, #6734, #20250, .T. ) ;
#5456 = APPROVAL_STATUS ( 'not_yet_approved' ) ;
#5457 = AXIS2_PLACEMENT_3D ( 'NONE', #1123, #13329, #2550 ) ;
#5458 = ORIENTED_EDGE ( 'NONE', *, *, #3562, .F. ) ;
#5459 = AXIS2_PLACEMENT_3D ( 'NONE', #2714, #8004, #9642 ) ;
#5460 = CARTESIAN_POINT ( 'NONE',  ( 57.14999999999999858, -3543.300000000000182, 2243.277199999999993 ) ) ;
#5461 = EDGE_LOOP ( 'NONE', ( #3204, #20639 ) ) ;
#5462 = DIRECTION ( 'NONE',  ( 0.000000000000000000, 0.000000000000000000, 1.000000000000000000 ) ) ;
#5463 = CYLINDRICAL_SURFACE ( 'NONE', #1467, 2.844800000000001550 ) ;
#5464 = EDGE_LOOP ( 'NONE', ( #9100, #15303, #6455, #14798 ) ) ;
#5465 = DIRECTION ( 'NONE',  ( 0.000000000000000000, 1.000000000000000000, 0.000000000000000000 ) ) ;
#5466 = B_SPLINE_CURVE_WITH_KNOTS ( 'NONE', 3,
 ( #12090, #10331, #10211, #15490, #4821, #17239 ),
 .UNSPECIFIED., .F., .F.,
 ( 4, 1, 1, 4 ),
 ( 0.000000000000000000, 0.3333333333333000081, 0.6666666666667000474, 1.000000000000000000 ),
 .UNSPECIFIED. ) ;
#5467 = CIRCLE ( 'NONE', #15932, 3.606799999999001027 ) ;
#5468 = CARTESIAN_POINT ( 'NONE',  ( 10.36831320293797276, -3578.148799999986750, 2239.391000000000076 ) ) ;
#5469 = CARTESIAN_POINT ( 'NONE',  ( 144.5623107343992331, -3576.491783798365759, 2245.815664034198562 ) ) ;
#5470 = DIRECTION ( 'NONE',  ( 0.000000000000000000, 0.000000000000000000, 1.000000000000000000 ) ) ;
#5471 = VECTOR ( 'NONE', #11791, 1000.000000000000000 ) ;
#5472 = CARTESIAN_POINT ( 'NONE',  ( 7.619999999999999218, -3599.497499999999945, 2296.591799999999694 ) ) ;
#5473 = APPROVAL ( #4561, 'UNKNOWN' ) ;
#5474 = AXIS2_PLACEMENT_3D ( 'NONE', #22814, #6902, #6785 ) ;
#5475 = FACE_OUTER_BOUND ( 'NONE', #17032, .T. ) ;
#5476 = AXIS2_PLACEMENT_3D ( 'NONE', #6908, #14053, #17669 ) ;
#5477 = ORIENTED_EDGE ( 'NONE', *, *, #13738, .T. ) ;
#5478 = DIRECTION ( 'NONE',  ( -0.8068916933244306700, 0.5906994119211842476, 0.000000000000000000 ) ) ;
#5479 = DIRECTION ( 'NONE',  ( 0.000000000000000000, 0.000000000000000000, 1.000000000000000000 ) ) ;
#5480 =( BOUNDED_CURVE ( )  B_SPLINE_CURVE ( 3, ( #17187, #13806, #8296, #1135 ),
 .UNSPECIFIED., .F., .T. ) 
 B_SPLINE_CURVE_WITH_KNOTS ( ( 4, 4 ),
 ( 1.570796327106734891, 3.141592653589766471 ),
 .UNSPECIFIED. ) 
 CURVE ( )  GEOMETRIC_REPRESENTATION_ITEM ( )  RATIONAL_B_SPLINE_CURVE ( ( 1.000000000000000000, 0.8047378541978723598, 0.8047378541978723598, 1.000000000000000000 ) ) 
 REPRESENTATION_ITEM ( '' )  );
#5481 = AXIS2_PLACEMENT_3D ( 'NONE', #17283, #2759, #22676 ) ;
#5482 = CARTESIAN_POINT ( 'NONE',  ( 15.41268679705191857, -3661.071170452636579, 2239.009999999999764 ) ) ;
#5483 = AXIS2_PLACEMENT_3D ( 'NONE', #11950, #12064, #3039 ) ;
#5484 = DIRECTION ( 'NONE',  ( 1.000000000000000000, -2.334777064353000131E-14, -2.343004830739999973E-14 ) ) ;
#5485 = CARTESIAN_POINT ( 'NONE',  ( 142.3802137133438350, -3543.693183278567176, 2255.422793245767480 ) ) ;
#5486 = VECTOR ( 'NONE', #21131, 1000.000000000000000 ) ;
#5487 = DIRECTION ( 'NONE',  ( -0.5000000000005969669, -0.8660254037840939834, 0.000000000000000000 ) ) ;
#5488 = B_SPLINE_CURVE_WITH_KNOTS ( 'NONE', 3,
 ( #15330, #19194, #11805, #6549, #11927, #8646, #6898, #1137, #13809, #3252, #10281, #4781, #1376, #11680, #22459, #13688, #6432, #13569, #20710 ),
 .UNSPECIFIED., .F., .F.,
 ( 4, 1, 1, 1, 1, 1, 1, 1, 1, 1, 1, 1, 1, 1, 1, 1, 4 ),
 ( 0.000000000000000000, 0.06250000000000000000, 0.1250000000000000000, 0.1875000000000000000, 0.2500000000000000000, 0.3125000000000000000, 0.3750000000000000000, 0.4375000000000000000, 0.5000000000000000000, 0.5625000000000000000, 0.6250000000000000000, 0.6875000000000000000, 0.7500000000000000000, 0.8125000000000000000, 0.8750000000000000000, 0.9375000000000000000, 0.9999968116805088014 ),
 .UNSPECIFIED. ) ;
#5489 = CARTESIAN_POINT ( 'NONE',  ( 7.518185888899349578, -3577.084101415800887, 2245.168125514048825 ) ) ;
#5490 = ORIENTED_EDGE ( 'NONE', *, *, #16082, .T. ) ;
#5491 = CARTESIAN_POINT ( 'NONE',  ( 127.0000000000000000, -3619.500000000000000, 2239.009999999999764 ) ) ;
#5492 = AXIS2_PLACEMENT_3D ( 'NONE', #11420, #6393, #4741 ) ;
#5493 = DIRECTION ( 'NONE',  ( -2.170301461641000033E-13, 1.295098308111999954E-13, -1.000000000000000000 ) ) ;
#5494 = AXIS2_PLACEMENT_3D ( 'NONE', #22304, #10467, #17369 ) ;
#5495 = PERSON_AND_ORGANIZATION_ROLE ( 'classification_officer' ) ;
#5496 = DIRECTION ( 'NONE',  ( 3.369279192186236859E-13, -1.000000000000000000, -5.827942386484301240E-13 ) ) ;
#5497 = AXIS2_PLACEMENT_3D ( 'NONE', #18975, #4550, #18849 ) ;
#5498 = DIRECTION ( 'NONE',  ( 0.000000000000000000, 0.000000000000000000, -1.000000000000000000 ) ) ;
#5499 = CARTESIAN_POINT ( 'NONE',  ( 16.87947181989943246, -3657.399155160218470, 2246.629991729495941 ) ) ;
#5500 = AXIS2_PLACEMENT_3D ( 'NONE', #7791, #20330, #14938 ) ;
#5501 = AXIS2_PLACEMENT_3D ( 'NONE', #20935, #4875, #23138 ) ;
#5502 = ORIENTED_EDGE ( 'NONE', *, *, #7294, .F. ) ;
#5503 = FACE_OUTER_BOUND ( 'NONE', #16844, .T. ) ;
#5504 = ORIENTED_EDGE ( 'NONE', *, *, #9872, .T. ) ;
#5505 = DIRECTION ( 'NONE',  ( 0.000000000000000000, 0.000000000000000000, -1.000000000000000000 ) ) ;
#5506 = APPLIED_DATE_AND_TIME_ASSIGNMENT ( #4237, #16423, ( #9636 ) ) ;
#5507 = CARTESIAN_POINT ( 'NONE',  ( 9.866773677518999364, -3639.188293979999798, 2279.450408114000311 ) ) ;
#5508 = ORIENTED_EDGE ( 'NONE', *, *, #21772, .T. ) ;
#5509 = CARTESIAN_POINT ( 'NONE',  ( 1.270000000000000018, -3660.140000000000327, 2247.392000000000280 ) ) ;
#5510 = AXIS2_PLACEMENT_3D ( 'NONE', #13502, #13161, #4261 ) ;
#5511 = EDGE_CURVE ( 'NONE', #10080, #9478, #17810, .T. ) ;
#5512 = ORIENTED_EDGE ( 'NONE', *, *, #14461, .F. ) ;
#5513 = FACE_OUTER_BOUND ( 'NONE', #7648, .T. ) ;
#5514 = DIRECTION ( 'NONE',  ( 1.000000000000000000, 0.000000000000000000, 0.000000000000000000 ) ) ;
#5515 = ADVANCED_FACE ( 'NONE', ( #5174 ), #19808, .T. ) ;
#5516 = ORIENTED_EDGE ( 'NONE', *, *, #18567, .F. ) ;
#5517 = ADVANCED_FACE ( 'NONE', ( #14307 ), #8795, .F. ) ;
#5518 = AXIS2_PLACEMENT_3D ( 'NONE', #8977, #5470, #12615 ) ;
#5519 = CARTESIAN_POINT ( 'NONE',  ( 137.2761739305270510, -3580.984189840409272, 2249.284302215166917 ) ) ;
#5520 = VECTOR ( 'NONE', #16073, 1000.000000000000000 ) ;
#5521 = ORIENTED_EDGE ( 'NONE', *, *, #3964, .T. ) ;
#5522 = DIRECTION ( 'NONE',  ( 0.000000000000000000, 0.000000000000000000, -1.000000000000000000 ) ) ;
#5523 = APPROVAL_DATE_TIME ( #17807, #3604 ) ;
#5524 = CARTESIAN_POINT ( 'NONE',  ( 142.1895021644337191, -3660.942314744887426, 2239.010000000037508 ) ) ;
#5525 = EDGE_CURVE ( 'NONE', #5448, #12925, #3740, .T. ) ;
#5526 = FACE_OUTER_BOUND ( 'NONE', #18737, .T. ) ;
#5527 = CARTESIAN_POINT ( 'NONE',  ( 151.1299999999999955, -3660.140000000000327, 2247.392000000000280 ) ) ;
#5528 = CIRCLE ( 'NONE', #14136, 1.269999999999993356 ) ;
#5529 = ADVANCED_FACE ( 'NONE', ( #21451 ), #19458, .T. ) ;
#5530 = CARTESIAN_POINT ( 'NONE',  ( 142.1475997075216924, -3578.044972006877742, 2250.117612943123277 ) ) ;
#5531 = VERTEX_POINT ( 'NONE', #7270 ) ;
#5532 = CARTESIAN_POINT ( 'NONE',  ( 134.8403290666279872, -3576.487559777513979, 2245.822145638164784 ) ) ;
#5533 = AXIS2_PLACEMENT_3D ( 'NONE', #21770, #2429, #10990 ) ;
#5534 = CIRCLE ( 'NONE', #10757, 5.460999999999938126 ) ;
#5535 = CARTESIAN_POINT ( 'NONE',  ( 136.8552000000001669, -3579.043785370568003, 2256.063560000000052 ) ) ;
#5536 = VERTEX_POINT ( 'NONE', #12424 ) ;
#5537 = VECTOR ( 'NONE', #8048, 1000.000000000000000 ) ;
#5538 = CARTESIAN_POINT ( 'NONE',  ( 15.54479999999999862, -3599.497499999999945, 2279.447335734999797 ) ) ;
#5539 = LINE ( 'NONE', #12781, #519 ) ;
#5540 = ORIENTED_EDGE ( 'NONE', *, *, #17533, .F. ) ;
#5541 = CARTESIAN_POINT ( 'NONE',  ( 15.21766708706000060, -3660.839381832000072, 2257.881320499000140 ) ) ;
#5542 = DIRECTION ( 'NONE',  ( 0.000000000000000000, 1.000000000000000000, 0.000000000000000000 ) ) ;
#5543 = EDGE_CURVE ( 'NONE', #15415, #7536, #5400, .T. ) ;
#5544 = EDGE_LOOP ( 'NONE', ( #13828, #14208, #18868, #18201 ) ) ;
#5545 = ADVANCED_FACE ( 'NONE', ( #9146 ), #9264, .T. ) ;
#5546 = LINE ( 'NONE', #144, #13581 ) ;
#5547 = CARTESIAN_POINT ( 'NONE',  ( 12.38525565295999975, -3642.335681406999811, 2279.814657614000225 ) ) ;
#5548 = SHAPE_REPRESENTATION_RELATIONSHIP ( 'NONE' , 'NONE' ,  #18056, #4892 ) ;
#5549 = DIRECTION ( 'NONE',  ( -0.8660254037839142383, -0.5000000000009082735, 0.000000000000000000 ) ) ;
#5550 = DIRECTION ( 'NONE',  ( -1.206643234470999950E-12, 1.000000000000000000, 0.000000000000000000 ) ) ;
#5551 = PERSON_AND_ORGANIZATION ( #5446, #1895 ) ;
#5552 = TOROIDAL_SURFACE ( 'NONE', #11509, 4.114799999999999791, 1.270000000000000018 ) ;
#5553 = CYLINDRICAL_SURFACE ( 'NONE', #649, 0.7619999999999294005 ) ;
#5554 = CARTESIAN_POINT ( 'NONE',  ( 35.56000000000000227, -3544.570000000000164, 2247.392000000000280 ) ) ;
#5555 = VERTEX_POINT ( 'NONE', #353 ) ;
#5556 = CARTESIAN_POINT ( 'NONE',  ( 18.22683998609632283, -3580.949329761737772, 2245.461031140869636 ) ) ;
#5557 = CARTESIAN_POINT ( 'NONE',  ( 137.8500712042239797, -3657.343683090691684, 2247.916757465596220 ) ) ;
#5558 = ORIENTED_EDGE ( 'NONE', *, *, #3248, .F. ) ;
#5559 = ORIENTED_EDGE ( 'NONE', *, *, #690, .F. ) ;
#5560 = CARTESIAN_POINT ( 'NONE',  ( 139.4325675808238145, -3662.349857698640790, 2249.183484300852342 ) ) ;
#5561 = AXIS2_PLACEMENT_3D ( 'NONE', #1409, #10549, #15601 ) ;
#5562 = VERTEX_POINT ( 'NONE', #11349 ) ;
#5563 = ORIENTED_EDGE ( 'NONE', *, *, #10070, .T. ) ;
#5564 = CARTESIAN_POINT ( 'NONE',  ( 57.14999999999999858, -3670.300000000000182, 2247.392000000000280 ) ) ;
#5565 = ORIENTED_EDGE ( 'NONE', *, *, #21012, .T. ) ;
#5566 = ORIENTED_EDGE ( 'NONE', *, *, #17727, .T. ) ;
#5567 = FACE_OUTER_BOUND ( 'NONE', #2385, .T. ) ;
#5568 = CALENDAR_DATE ( 2026, 26, 10 ) ;
#5569 = DIRECTION ( 'NONE',  ( 0.000000000000000000, 0.000000000000000000, -1.000000000000000000 ) ) ;
#5570 = DIRECTION ( 'NONE',  ( -1.000000000000000000, 0.000000000000000000, 0.000000000000000000 ) ) ;
#5571 = EDGE_LOOP ( 'NONE', ( #305, #11250, #6356, #1585, #18887, #22121, #12980, #4194, #8219, #6390 ) ) ;
#5572 = CARTESIAN_POINT ( 'NONE',  ( 0.000000000000000000, -3544.061999999999898, 2253.487999999999829 ) ) ;
#5573 = PLANE ( 'NONE',  #22060 ) ;
#5574 = DIRECTION ( 'NONE',  ( 1.000000000000000000, 0.000000000000000000, 0.000000000000000000 ) ) ;
#5575 = FACE_OUTER_BOUND ( 'NONE', #8891, .T. ) ;
#5576 = DATE_TIME_ROLE ( 'classification_date' ) ;
#5577 = EDGE_CURVE ( 'NONE', #12211, #10812, #13354, .T. ) ;
#5578 = ORIENTED_EDGE ( 'NONE', *, *, #16821, .T. ) ;
#5579 = CARTESIAN_POINT ( 'NONE',  ( 131.7018428614628931, -3543.338148339810232, 2259.652932710757341 ) ) ;
#5580 = ADVANCED_FACE ( 'NONE', ( #14887 ), #985, .T. ) ;
#5581 = ORIENTED_EDGE ( 'NONE', *, *, #4085, .F. ) ;
#5582 = TOROIDAL_SURFACE ( 'NONE', #18649, 7.112000000000000099, 0.7620000000000000107 ) ;
#5583 = FACE_OUTER_BOUND ( 'NONE', #22416, .T. ) ;
#5584 = CARTESIAN_POINT ( 'NONE',  ( 7.881367952664562360, -3662.577932297246662, 2245.924867616539359 ) ) ;
#5585 = EDGE_CURVE ( 'NONE', #10080, #22988, #12241, .T. ) ;
#5586 = EDGE_LOOP ( 'NONE', ( #12495, #4334, #10300, #8317 ) ) ;
#5587 = DIRECTION ( 'NONE',  ( -0.6887494619146010688, 0.000000000000000000, -0.7249994335945012525 ) ) ;
#5588 = CARTESIAN_POINT ( 'NONE',  ( 12.69997932225824400, -3596.652698770999905, 2279.817639835496266 ) ) ;
#5589 = DIRECTION ( 'NONE',  ( 0.000000000000000000, -1.000000000000000000, 0.000000000000000000 ) ) ;
#5590 = ADVANCED_FACE ( 'NONE', ( #9602 ), #22233, .F. ) ;
#5591 = CARTESIAN_POINT ( 'NONE',  ( 35.56000000000000227, -3568.700000000000273, 2244.547199999999975 ) ) ;
#5592 = EDGE_LOOP ( 'NONE', ( #20136, #2501, #2330, #14997 ) ) ;
#5593 = ADVANCED_FACE ( 'NONE', ( #20270 ), #18388, .F. ) ;
#5594 = LINE ( 'NONE', #17998, #11081 ) ;
#5595 = VERTEX_POINT ( 'NONE', #465 ) ;
#5596 = CARTESIAN_POINT ( 'NONE',  ( 129.8447999999989975, -3619.500000000000000, 2259.837999999999738 ) ) ;
#5597 = DIRECTION ( 'NONE',  ( 5.432398939370942693E-28, 1.000000000000000000, 2.336881798971000105E-14 ) ) ;
#5598 = AXIS2_PLACEMENT_3D ( 'NONE', #5830, #4054, #18578 ) ;
#5599 = FACE_OUTER_BOUND ( 'NONE', #12527, .T. ) ;
#5600 = DIRECTION ( 'NONE',  ( 0.000000000000000000, 0.000000000000000000, -1.000000000000000000 ) ) ;
#5601 = DIRECTION ( 'NONE',  ( -0.8660254037840939834, 0.5000000000005969669, 0.000000000000000000 ) ) ;
#5602 = CARTESIAN_POINT ( 'NONE',  ( 7.485436129649806425, -3577.156296306550303, 2245.113781002514770 ) ) ;
#5603 = EDGE_LOOP ( 'NONE', ( #6962, #6406 ) ) ;
#5604 = PERSON_AND_ORGANIZATION_ROLE ( 'classification_officer' ) ;
#5605 = DIRECTION ( 'NONE',  ( 0.000000000000000000, 0.000000000000000000, -1.000000000000000000 ) ) ;
#5606 = CARTESIAN_POINT ( 'NONE',  ( 9.989231719078535576, -3543.619369469922731, 2255.346378162066230 ) ) ;
#5607 = ITEM_DEFINED_TRANSFORMATION ( 'NONE', 'NONE', #21711,  #5611 ) ;
#5608 = AXIS2_PLACEMENT_3D ( 'NONE', #2756, #12367, #10728 ) ;
#5609 = DIRECTION ( 'NONE',  ( -2.848812946084999742E-12, -1.000000000000000000, 0.000000000000000000 ) ) ;
#5610 = DIRECTION ( 'NONE',  ( -1.000000000000000000, 0.000000000000000000, 0.000000000000000000 ) ) ;
#5611 = AXIS2_PLACEMENT_3D ( 'NONE', #2606, #9751, #7545 ) ;
#5612 = FACE_OUTER_BOUND ( 'NONE', #13407, .T. ) ;
#5613 = ORIENTED_EDGE ( 'NONE', *, *, #20733, .F. ) ;
#5614 = CYLINDRICAL_SURFACE ( 'NONE', #16266, 0.7619999999999294005 ) ;
#5615 = ORIENTED_EDGE ( 'NONE', *, *, #17292, .F. ) ;
#5616 =( BOUNDED_CURVE ( )  B_SPLINE_CURVE ( 3, ( #19456, #5524, #17808, #12655 ),
 .UNSPECIFIED., .F., .F. ) 
 B_SPLINE_CURVE_WITH_KNOTS ( ( 4, 4 ),
 ( 1.570796326964226219, 3.141592653589766471 ),
 .UNSPECIFIED. ) 
 CURVE ( )  GEOMETRIC_REPRESENTATION_ITEM ( )  RATIONAL_B_SPLINE_CURVE ( ( 1.000000000000000000, 0.8047378541642826733, 0.8047378541642826733, 1.000000000000000000 ) ) 
 REPRESENTATION_ITEM ( '' )  );
#5617 = CYLINDRICAL_SURFACE ( 'NONE', #12577, 5.715000000000001634 ) ;
#5618 = CARTESIAN_POINT ( 'NONE',  ( 10.92571717110000051, -3637.270967911999833, 2279.676081828000406 ) ) ;
#5619 = ORIENTED_EDGE ( 'NONE', *, *, #12505, .F. ) ;
#5620 = CARTESIAN_POINT ( 'NONE',  ( 19.05000000000000071, -3658.235000000000127, 2247.392000000000280 ) ) ;
#5621 = CIRCLE ( 'NONE', #13840, 2.844799999999961582 ) ;
#5622 = ORIENTED_EDGE ( 'NONE', *, *, #10979, .T. ) ;
#5623 = CARTESIAN_POINT ( 'NONE',  ( 142.5446907139761663, -3695.594480551361812, 2255.010836426532023 ) ) ;
#5624 = FACE_OUTER_BOUND ( 'NONE', #1938, .T. ) ;
#5625 = LOCAL_TIME ( 17, 37, 43.00000000000000000, #2937 ) ;
#5626 = ORIENTED_EDGE ( 'NONE', *, *, #12161, .T. ) ;
#5627 = CARTESIAN_POINT ( 'NONE',  ( 137.9085718133126761, -3581.704955524434354, 2247.466441185878466 ) ) ;
#5628 = VERTEX_POINT ( 'NONE', #4211 ) ;
#5629 = CARTESIAN_POINT ( 'NONE',  ( 6.223000000000999066, -3599.497499999999945, 2296.591799999999694 ) ) ;
#5630 = APPROVAL_DATE_TIME ( #3977, #7348 ) ;
#5631 = APPROVAL ( #21447, 'UNSPECIFIED' ) ;
#5632 = CARTESIAN_POINT ( 'NONE',  ( 15.48106116729000092, -3640.128614708000441, 2279.464089926999804 ) ) ;
#5633 = CARTESIAN_POINT ( 'NONE',  ( 0.7620000000000000107, -3695.699999999999818, 2275.763800000000174 ) ) ;
#5634 = AXIS2_PLACEMENT_3D ( 'NONE', #18589, #13084, #14962 ) ;
#5635 = DIRECTION ( 'NONE',  ( 1.000000000000000000, 0.000000000000000000, 0.000000000000000000 ) ) ;
#5636 = DIRECTION ( 'NONE',  ( 0.000000000000000000, 0.000000000000000000, 1.000000000000000000 ) ) ;
#5637 = EDGE_CURVE ( 'NONE', #4904, #14376, #17190, .T. ) ;
#5638 = APPLIED_APPROVAL_ASSIGNMENT ( #18779, ( #15652 ) ) ;
#5639 = CARTESIAN_POINT ( 'NONE',  ( 141.2946836820506746, -3577.137378286903640, 2249.656812253273529 ) ) ;
#5640 = ORIENTED_EDGE ( 'NONE', *, *, #18398, .F. ) ;
#5641 =( GEOMETRIC_REPRESENTATION_CONTEXT ( 3 ) GLOBAL_UNCERTAINTY_ASSIGNED_CONTEXT ( ( #22120 ) ) GLOBAL_UNIT_ASSIGNED_CONTEXT ( ( #7866, #11370, #22034 ) ) REPRESENTATION_CONTEXT ( 'NONE', 'WORKASPACE' ) );
#5642 = CARTESIAN_POINT ( 'NONE',  ( 134.7909367546303088, -3576.568141679416840, 2245.704773985674819 ) ) ;
#5643 = EDGE_CURVE ( 'NONE', #21665, #14933, #11574, .T. ) ;
#5644 = ORIENTED_EDGE ( 'NONE', *, *, #8538, .T. ) ;
#5645 = CARTESIAN_POINT ( 'NONE',  ( -12.31900000000000084, -3661.486200000000281, 2245.060313203000078 ) ) ;
#5646 = DIRECTION ( 'NONE',  ( 0.000000000000000000, 0.000000000000000000, -1.000000000000000000 ) ) ;
#5647 = VERTEX_POINT ( 'NONE', #22016 ) ;
#5648 = LINE ( 'NONE', #19939, #1941 ) ;
#5649 = CARTESIAN_POINT ( 'NONE',  ( 64.76999999999999602, -3670.300000000000182, 2289.213099999999940 ) ) ;
#5650 = VERTEX_POINT ( 'NONE', #21908 ) ;
#5651 = CARTESIAN_POINT ( 'NONE',  ( 12.69999999996000106, -3642.194899999999961, 2292.781800000000203 ) ) ;
#5652 = CARTESIAN_POINT ( 'NONE',  ( -0.7620000000000000107, -3660.140000000000327, 2250.998800000000301 ) ) ;
#5653 = CARTESIAN_POINT ( 'NONE',  ( 0.000000000000000000, 0.000000000000000000, 0.000000000000000000 ) ) ;
#5654 = APPLIED_APPROVAL_ASSIGNMENT ( #16776, ( #12016 ) ) ;
#5655 = CARTESIAN_POINT ( 'NONE',  ( -5.588000000000000078, -3578.860000000000127, 2243.785200000000259 ) ) ;
#5656 = LOCAL_TIME ( 17, 37, 43.00000000000000000, #7465 ) ;
#5657 = DIRECTION ( 'NONE',  ( 0.000000000000000000, 0.000000000000000000, -1.000000000000000000 ) ) ;
#5658 = COORDINATED_UNIVERSAL_TIME_OFFSET ( 0, 0, .AHEAD. ) ;
#5659 = EDGE_LOOP ( 'NONE', ( #6169, #21626, #5062, #18100 ) ) ;
#5660 = CARTESIAN_POINT ( 'NONE',  ( 6.984999999999000231, -3579.494999999999891, 2239.771999999999935 ) ) ;
#5661 = ORIENTED_EDGE ( 'NONE', *, *, #7003, .T. ) ;
#5662 = DIRECTION ( 'NONE',  ( 3.101153370604999976E-13, -3.885294924346999989E-13, -1.000000000000000000 ) ) ;
#5663 = CARTESIAN_POINT ( 'NONE',  ( 137.8060722392503124, -3657.382237692640956, 2248.090672303196698 ) ) ;
#5664 = CIRCLE ( 'NONE', #18735, 0.7619999999999294005 ) ;
#5665 = EDGE_CURVE ( 'NONE', #140, #22588, #10735, .T. ) ;
#5666 = ORIENTED_EDGE ( 'NONE', *, *, #4610, .F. ) ;
#5667 = ORIENTED_EDGE ( 'NONE', *, *, #5945, .T. ) ;
#5668 = ADVANCED_FACE ( 'NONE', ( #5873 ), #13010, .T. ) ;
#5669 = CARTESIAN_POINT ( 'NONE',  ( 137.5443672346975745, -3661.361536096956115, 2249.961261516084505 ) ) ;
#5670 = ADVANCED_FACE ( 'NONE', ( #16623 ), #9254, .T. ) ;
#5671 = ORIENTED_EDGE ( 'NONE', *, *, #11946, .T. ) ;
#5672 = APPLIED_SECURITY_CLASSIFICATION_ASSIGNMENT ( #2304, ( #23178 ) ) ;
#5673 = ORIENTED_EDGE ( 'NONE', *, *, #22385, .T. ) ;
#5674 = DIRECTION ( 'NONE',  ( -1.159746789737949940E-14, -0.5000000000004778400, 0.8660254037841628172 ) ) ;
#5675 = ORIENTED_EDGE ( 'NONE', *, *, #7526, .F. ) ;
#5676 = ORIENTED_EDGE ( 'NONE', *, *, #1557, .T. ) ;
#5677 = CARTESIAN_POINT ( 'NONE',  ( 15.54479999999999862, -3659.504999999999654, 2256.063560000000052 ) ) ;
#5678 = DATE_AND_TIME ( #4028, #3778 ) ;
#5679 = DIRECTION ( 'NONE',  ( -1.000000000000000000, 0.000000000000000000, 0.000000000000000000 ) ) ;
#5680 = CIRCLE ( 'NONE', #7178, 6.349999999999855760 ) ;
#5681 = ORIENTED_EDGE ( 'NONE', *, *, #21985, .T. ) ;
#5682 = AXIS2_PLACEMENT_3D ( 'NONE', #6136, #18430, #9862 ) ;
#5683 = DIRECTION ( 'NONE',  ( -5.461016542361937364E-28, 1.000000000000000000, -2.336881798971000105E-14 ) ) ;
#5684 = ORIENTED_EDGE ( 'NONE', *, *, #5800, .F. ) ;
#5685 = FACE_BOUND ( 'NONE', #178, .T. ) ;
#5686 = CARTESIAN_POINT ( 'NONE',  ( 7.161827360861991565, -3580.901497745790039, 2245.410526384100649 ) ) ;
#5687 = EDGE_CURVE ( 'NONE', #22803, #11827, #6206, .T. ) ;
#5688 = CARTESIAN_POINT ( 'NONE',  ( -6.731000000000127770, -3665.601000000000113, 2247.392000000000280 ) ) ;
#5689 = CALENDAR_DATE ( 2026, 26, 10 ) ;
#5690 = CARTESIAN_POINT ( 'NONE',  ( 131.7495946018047164, -3543.379535511729046, 2259.772542604667706 ) ) ;
#5691 = ORIENTED_EDGE ( 'NONE', *, *, #20167, .F. ) ;
#5692 = CARTESIAN_POINT ( 'NONE',  ( 114.2999999999999972, -3594.099999999999909, 2239.771999999999935 ) ) ;
#5693 = DIRECTION ( 'NONE',  ( -1.000000000000000000, 0.000000000000000000, 0.000000000000000000 ) ) ;
#5694 = CARTESIAN_POINT ( 'NONE',  ( -12.69999999999999929, -3660.140000000000327, 2247.392000000000280 ) ) ;
#5695 = ORIENTED_EDGE ( 'NONE', *, *, #1195, .T. ) ;
#5696 = AXIS2_PLACEMENT_3D ( 'NONE', #18214, #64, #15884 ) ;
#5697 = SPHERICAL_SURFACE ( 'NONE', #5123, 1.270000000000000018 ) ;
#5698 = EDGE_CURVE ( 'NONE', #8438, #698, #15543, .T. ) ;
#5699 = CIRCLE ( 'NONE', #89, 0.7619999999999987894 ) ;
#5700 = DIRECTION ( 'NONE',  ( 0.000000000000000000, 0.000000000000000000, 1.000000000000000000 ) ) ;
#5701 = DIRECTION ( 'NONE',  ( 1.000000000000000000, 0.000000000000000000, 0.000000000000000000 ) ) ;
#5702 = LINE ( 'NONE', #18108, #10271 ) ;
#5703 = ORIENTED_EDGE ( 'NONE', *, *, #9981, .F. ) ;
#5704 = EDGE_CURVE ( 'NONE', #15378, #6511, #23063, .T. ) ;
#5705 = ADVANCED_FACE ( 'NONE', ( #793 ), #4740, .T. ) ;
#5706 = CYLINDRICAL_SURFACE ( 'NONE', #6590, 2.844800000000091700 ) ;
#5707 = ORIENTED_EDGE ( 'NONE', *, *, #3137, .T. ) ;
#5708 = CARTESIAN_POINT ( 'NONE',  ( 147.7417438321762404, -3695.684722677512127, 2259.544515782609324 ) ) ;
#5709 = CARTESIAN_POINT ( 'NONE',  ( 17.78000000000000114, -3579.494999999999891, 2239.391000000000076 ) ) ;
#5710 = TOROIDAL_SURFACE ( 'NONE', #19178, 3.606799999999999784, 0.7620000000000000107 ) ;
#5711 = DIRECTION ( 'NONE',  ( 0.8660254037826368156, 0.5000000000031208369, 0.000000000000000000 ) ) ;
#5712 = CARTESIAN_POINT ( 'NONE',  ( -6.349999999999999645, -3694.938000000000102, 2229.612000000000080 ) ) ;
#5713 = CARTESIAN_POINT ( 'NONE',  ( 142.2521676912461999, -3544.290797605575335, 2255.743587683598435 ) ) ;
#5714 = CARTESIAN_POINT ( 'NONE',  ( 10.36831320283000046, -3600.843699999999899, 2292.781800000000203 ) ) ;
#5715 = AXIS2_PLACEMENT_3D ( 'NONE', #5655, #12790, #374 ) ;
#5716 = ADVANCED_FACE ( 'NONE', ( #4439 ), #1142, .T. ) ;
#5717 = AXIS2_PLACEMENT_3D ( 'NONE', #16083, #7183, #14336 ) ;
#5718 = CARTESIAN_POINT ( 'NONE',  ( 7.139750157027973110, -3578.173783392149744, 2244.630952135868938 ) ) ;
#5719 = ORIENTED_EDGE ( 'NONE', *, *, #15246, .F. ) ;
#5720 = DATE_AND_TIME ( #20978, #4141 ) ;
#5721 = AXIS2_PLACEMENT_3D ( 'NONE', #567, #14873, #2658 ) ;
#5722 = CARTESIAN_POINT ( 'NONE',  ( -12.31899999999994755, -3657.447599999831709, 2247.391999999993914 ) ) ;
#5723 = CARTESIAN_POINT ( 'NONE',  ( 12.69999999999999929, -3642.677500000000236, 2264.841800000000148 ) ) ;
#5724 = APPROVAL_DATE_TIME ( #21765, #16488 ) ;
#5725 = EDGE_CURVE ( 'NONE', #10346, #5746, #3023, .T. ) ;
#5726 = CARTESIAN_POINT ( 'NONE',  ( 101.5999999999999943, -3568.700000000000273, 2239.009999999999764 ) ) ;
#5727 = ADVANCED_FACE ( 'NONE', ( #22815 ), #10169, .F. ) ;
#5728 = DIRECTION ( 'NONE',  ( -0.8660254037843172492, 0.5000000000002102762, 3.628718844336076700E-12 ) ) ;
#5729 = ORIENTED_EDGE ( 'NONE', *, *, #17685, .F. ) ;
#5730 = AXIS2_PLACEMENT_3D ( 'NONE', #18418, #4357, #11496 ) ;
#5731 = CARTESIAN_POINT ( 'NONE',  ( 134.9402830941174898, -3662.669251256681946, 2246.087205945077585 ) ) ;
#5732 = CARTESIAN_POINT ( 'NONE',  ( 25.39999999999999858, -3660.140000000000327, 2247.392000000000280 ) ) ;
#5733 = ORIENTED_EDGE ( 'NONE', *, *, #8969, .T. ) ;
#5734 = AXIS2_PLACEMENT_3D ( 'NONE', #1339, #19395, #19276 ) ;
#5735 = CARTESIAN_POINT ( 'NONE',  ( 12.69999999999999929, -3579.494999999999891, 2272.030000000000200 ) ) ;
#5736 = CIRCLE ( 'NONE', #15453, 0.7619999999999987894 ) ;
#5737 = EDGE_CURVE ( 'NONE', #4127, #16752, #14434, .T. ) ;
#5738 = DIRECTION ( 'NONE',  ( 0.000000000000000000, -1.000000000000000000, 0.000000000000000000 ) ) ;
#5739 = ORIENTED_EDGE ( 'NONE', *, *, #17583, .T. ) ;
#5740 = CARTESIAN_POINT ( 'NONE',  ( 17.78000000000000114, -3579.494999999999891, 2244.978999999999814 ) ) ;
#5741 = VECTOR ( 'NONE', #17274, 1000.000000000000000 ) ;
#5742 = ORIENTED_EDGE ( 'NONE', *, *, #7816, .F. ) ;
#5743 = CARTESIAN_POINT ( 'NONE',  ( 142.3294809625096775, -3695.151712724517893, 2255.549776698367168 ) ) ;
#5744 = CARTESIAN_POINT ( 'NONE',  ( 139.6999999999999886, -3579.494999999999891, 2244.978999999999814 ) ) ;
#5745 = AXIS2_PLACEMENT_3D ( 'NONE', #22708, #4788, #6438 ) ;
#5746 = VERTEX_POINT ( 'NONE', #16967 ) ;
#5747 = CARTESIAN_POINT ( 'NONE',  ( 137.8998175441851686, -3581.697724730667233, 2247.187286018316172 ) ) ;
#5748 = UNCERTAINTY_MEASURE_WITH_UNIT (LENGTH_MEASURE( 1.000000000000000082E-05 ), #9985, 'distance_accuracy_value', 'NONE');
#5749 = ORIENTED_EDGE ( 'NONE', *, *, #18697, .T. ) ;
#5750 = CARTESIAN_POINT ( 'NONE',  ( 145.4149999194000316, -3579.609095813974363, 2244.645121672132518 ) ) ;
#5751 = CALENDAR_DATE ( 2026, 26, 10 ) ;
#5752 = EDGE_CURVE ( 'NONE', #18880, #452, #11932, .T. ) ;
#5753 = CIRCLE ( 'NONE', #9123, 5.460999999999938126 ) ;
#5754 = FACE_OUTER_BOUND ( 'NONE', #10645, .T. ) ;
#5755 = FACE_OUTER_BOUND ( 'NONE', #2021, .T. ) ;
#5756 = DIRECTION ( 'NONE',  ( 1.000000000000000000, 4.457711412217000029E-12, 2.901972884401000201E-13 ) ) ;
#5757 = DIRECTION ( 'NONE',  ( 0.000000000000000000, 0.000000000000000000, -1.000000000000000000 ) ) ;
#5758 = CARTESIAN_POINT ( 'NONE',  ( 137.9912716215963542, -3577.220450210613308, 2249.716878566800460 ) ) ;
#5759 = EDGE_LOOP ( 'NONE', ( #21581, #14386, #3273, #19353 ) ) ;
#5760 = VECTOR ( 'NONE', #21739, 1000.000000000000000 ) ;
#5761 = CARTESIAN_POINT ( 'NONE',  ( 134.3629476791235504, -3577.447007153130926, 2244.917889002162610 ) ) ;
#5762 = AXIS2_PLACEMENT_3D ( 'NONE', #12627, #18347, #14850 ) ;
#5763 = CARTESIAN_POINT ( 'NONE',  ( 12.69999999999999929, -3659.504999999999654, 2245.359999999999673 ) ) ;
#5764 = ORIENTED_EDGE ( 'NONE', *, *, #10063, .T. ) ;
#5765 = FACE_OUTER_BOUND ( 'NONE', #9925, .T. ) ;
#5766 = DIRECTION ( 'NONE',  ( 0.000000000000000000, -1.000000000000000000, 0.000000000000000000 ) ) ;
#5767 = VECTOR ( 'NONE', #7836, 1000.000000000000000 ) ;
#5768 = CIRCLE ( 'NONE', #13611, 1.269999999999882334 ) ;
#5769 = ORIENTED_EDGE ( 'NONE', *, *, #15533, .T. ) ;
#5770 = CARTESIAN_POINT ( 'NONE',  ( 13.24911585008999815, -3662.300876935000360, 2257.605101898000157 ) ) ;
#5771 = CARTESIAN_POINT ( 'NONE',  ( 11.47173590547000011, -3596.924856509000165, 2279.750831905999803 ) ) ;
#5772 = ORIENTED_EDGE ( 'NONE', *, *, #1236, .F. ) ;
#5773 = CARTESIAN_POINT ( 'NONE',  ( 50.79999999999999716, -3568.700000000000273, 2259.837999999999738 ) ) ;
#5774 = DIRECTION ( 'NONE',  ( -0.8660254037817187722, 0.5000000000047108983, 0.000000000000000000 ) ) ;
#5775 = CARTESIAN_POINT ( 'NONE',  ( 50.79999999999999716, -3670.300000000000182, 2261.869999999999891 ) ) ;
#5776 = EDGE_LOOP ( 'NONE', ( #10627, #9894 ) ) ;
#5777 = CARTESIAN_POINT ( 'NONE',  ( 127.0000000000000000, -3670.300000000000182, 2259.837999999999738 ) ) ;
#5778 = CIRCLE ( 'NONE', #1265, 2.844800000000091700 ) ;
#5779 = COORDINATED_UNIVERSAL_TIME_OFFSET ( 0, 0, .AHEAD. ) ;
#5780 = CIRCLE ( 'NONE', #18851, 5.460999999999938126 ) ;
#5781 = CARTESIAN_POINT ( 'NONE',  ( 139.6999999999999886, -3579.494999999999891, 2239.771999999999935 ) ) ;
#5782 = CARTESIAN_POINT ( 'NONE',  ( 9.923473159618289685, -3578.875297092680739, 2250.236699640666302 ) ) ;
#5783 = ORIENTED_EDGE ( 'NONE', *, *, #15254, .T. ) ;
#5784 = CARTESIAN_POINT ( 'NONE',  ( 18.26250405562707613, -3580.806353043069066, 2245.317242612439259 ) ) ;
#5785 = DIRECTION ( 'NONE',  ( 0.000000000000000000, 0.000000000000000000, -1.000000000000000000 ) ) ;
#5786 = ORIENTED_EDGE ( 'NONE', *, *, #1509, .F. ) ;
#5787 = CARTESIAN_POINT ( 'NONE',  ( 137.2524928180403947, -3660.955183479468360, 2250.117566548333343 ) ) ;
#5788 = ORIENTED_EDGE ( 'NONE', *, *, #9373, .F. ) ;
#5789 = VERTEX_POINT ( 'NONE', #8546 ) ;
#5790 = CIRCLE ( 'NONE', #13259, 3.175000000000149925 ) ;
#5791 = APPROVAL ( #19398, 'UNSPECIFIED' ) ;
#5792 = CARTESIAN_POINT ( 'NONE',  ( 57.14999999999999858, -3694.430000000000291, 2247.392000000000280 ) ) ;
#5793 = AXIS2_PLACEMENT_3D ( 'NONE', #3121, #12381, #1475 ) ;
#5794 = ORIENTED_EDGE ( 'NONE', *, *, #8642, .F. ) ;
#5795 = DIRECTION ( 'NONE',  ( -1.073225997510925892E-13, 0.000000000000000000, -1.000000000000000000 ) ) ;
#5796 = SECURITY_CLASSIFICATION_LEVEL ( 'unclassified' ) ;
#5797 = CARTESIAN_POINT ( 'NONE',  ( 12.69999999999999929, -3659.504999999999654, 2246.630000000000109 ) ) ;
#5798 = EDGE_LOOP ( 'NONE', ( #19616, #8244, #11886, #16263, #8019 ) ) ;
#5799 = CARTESIAN_POINT ( 'NONE',  ( 0.7620000000000000107, -3694.938000000000102, 2275.763800000000174 ) ) ;
#5800 = EDGE_CURVE ( 'NONE', #7394, #15975, #4377, .T. ) ;
#5801 =( LENGTH_UNIT ( ) NAMED_UNIT ( * ) SI_UNIT ( .MILLI., .METRE. ) );
#5802 = CARTESIAN_POINT ( 'NONE',  ( 7.149936657841415411, -3580.855533714582634, 2245.364243621501828 ) ) ;
#5803 = ADVANCED_FACE ( 'NONE', ( #15335 ), #15970, .T. ) ;
#5804 = DIRECTION ( 'NONE',  ( -1.224646799147353207E-16, 1.000000000000000000, 0.000000000000000000 ) ) ;
#5805 = PERSON_AND_ORGANIZATION ( #5446, #1895 ) ;
#5806 = EDGE_CURVE ( 'NONE', #12349, #6304, #5883, .T. ) ;
#5807 = FACE_OUTER_BOUND ( 'NONE', #17476, .T. ) ;
#5808 = ORIENTED_EDGE ( 'NONE', *, *, #6706, .T. ) ;
#5809 = VECTOR ( 'NONE', #14895, 1000.000000000000000 ) ;
#5810 = CIRCLE ( 'NONE', #1673, 2.844800000000001550 ) ;
#5811 = DIRECTION ( 'NONE',  ( 1.000000000000000000, -0.000000000000000000, -0.000000000000000000 ) ) ;
#5812 = ORIENTED_EDGE ( 'NONE', *, *, #5208, .F. ) ;
#5813 = CARTESIAN_POINT ( 'NONE',  ( 7.361549341673686797, -3661.582738350905856, 2244.919123108159965 ) ) ;
#5814 = AXIS2_PLACEMENT_3D ( 'NONE', #3557, #10712, #15268 ) ;
#5815 = EDGE_CURVE ( 'NONE', #17789, #8413, #6051, .T. ) ;
#5816 = EDGE_CURVE ( 'NONE', #16978, #17829, #6631, .T. ) ;
#5817 = ORIENTED_EDGE ( 'NONE', *, *, #776, .T. ) ;
#5818 = EDGE_CURVE ( 'NONE', #18205, #17996, #22699, .T. ) ;
#5819 = DIRECTION ( 'NONE',  ( -2.324635735433000053E-14, 2.336881798971000105E-14, -1.000000000000000000 ) ) ;
#5820 = CARTESIAN_POINT ( 'NONE',  ( -5.588000000000000078, -3694.938000000000102, 2253.487999999999829 ) ) ;
#5821 = CARTESIAN_POINT ( 'NONE',  ( 55.57575231171000496, -3544.061999999999898, 2275.763800000000174 ) ) ;
#5822 = ORIENTED_EDGE ( 'NONE', *, *, #4996, .F. ) ;
#5823 = DIRECTION ( 'NONE',  ( -1.000000000000000000, 0.000000000000000000, 0.000000000000000000 ) ) ;
#5824 = ORIENTED_EDGE ( 'NONE', *, *, #21053, .T. ) ;
#5825 = LINE ( 'NONE', #12842, #2742 ) ;
#5826 = DIRECTION ( 'NONE',  ( 1.000000000000000000, 0.000000000000000000, 0.000000000000000000 ) ) ;
#5827 = AXIS2_PLACEMENT_3D ( 'NONE', #18281, #21913, #7398 ) ;
#5828 = DIRECTION ( 'NONE',  ( 0.000000000000000000, 0.000000000000000000, 1.000000000000000000 ) ) ;
#5829 = VECTOR ( 'NONE', #19092, 1000.000000000000000 ) ;
#5830 = CARTESIAN_POINT ( 'NONE',  ( 3.048000000000000043, -3694.938000000000102, 2238.248000000000047 ) ) ;
#5831 = AXIS2_PLACEMENT_3D ( 'NONE', #2387, #16668, #6480 ) ;
#5832 = DIRECTION ( 'NONE',  ( 0.000000000000000000, 0.000000000000000000, -1.000000000000000000 ) ) ;
#5833 = DIRECTION ( 'NONE',  ( -1.000000000000000000, -2.848935406719999894E-12, 0.000000000000000000 ) ) ;
#5834 = CARTESIAN_POINT ( 'NONE',  ( 129.8447999999989975, -3670.300000000000182, 2239.771999999999935 ) ) ;
#5835 = ORIENTED_EDGE ( 'NONE', *, *, #18028, .T. ) ;
#5836 = PRODUCT_CONTEXT ( 'NONE', #9618, 'mechanical' ) ;
#5837 = ADVANCED_FACE ( 'NONE', ( #22467 ), #13696, .T. ) ;
#5838 = MANIFOLD_SOLID_BREP ( 'SOLID2-15[1]', #16587 ) ;
#5839 = VERTEX_POINT ( 'NONE', #4787 ) ;
#5840 = CARTESIAN_POINT ( 'NONE',  ( 145.4114887792144373, -3659.274894571976347, 2244.679117411749758 ) ) ;
#5841 = EDGE_CURVE ( 'NONE', #14892, #14824, #16035, .T. ) ;
#5842 = CARTESIAN_POINT ( 'NONE',  ( 17.78000000000000114, -3639.502500000000055, 2296.591799999999694 ) ) ;
#5843 = ADVANCED_FACE ( 'NONE', ( #1492 ), #10634, .T. ) ;
#5844 = DIRECTION ( 'NONE',  ( 1.000000000000000000, 0.000000000000000000, 0.000000000000000000 ) ) ;
#5845 = AXIS2_PLACEMENT_3D ( 'NONE', #1951, #537, #3936 ) ;
#5846 = ORIENTED_EDGE ( 'NONE', *, *, #15729, .F. ) ;
#5847 = VECTOR ( 'NONE', #21321, 1000.000000000000000 ) ;
#5848 = CYLINDRICAL_SURFACE ( 'NONE', #16737, 2.844800000000091700 ) ;
#5849 = AXIS2_PLACEMENT_3D ( 'NONE', #4443, #11579, #915 ) ;
#5850 = ORIENTED_EDGE ( 'NONE', *, *, #3636, .F. ) ;
#5851 = DIRECTION ( 'NONE',  ( 0.7249994335945985080, 0.000000000000000000, -0.6887494619144985952 ) ) ;
#5852 = ORIENTED_EDGE ( 'NONE', *, *, #9548, .F. ) ;
#5853 = DIRECTION ( 'NONE',  ( 0.000000000000000000, 0.000000000000000000, 1.000000000000000000 ) ) ;
#5854 = EDGE_LOOP ( 'NONE', ( #20497, #17861, #8388, #18404, #20486, #17643 ) ) ;
#5855 = EDGE_CURVE ( 'NONE', #8104, #4940, #14122, .T. ) ;
#5856 = FACE_OUTER_BOUND ( 'NONE', #6335, .T. ) ;
#5857 = ORIENTED_EDGE ( 'NONE', *, *, #7508, .F. ) ;
#5858 = CARTESIAN_POINT ( 'NONE',  ( 12.69999999999999929, -3579.494999999999891, 2239.391000000000076 ) ) ;
#5859 = CYLINDRICAL_SURFACE ( 'NONE', #21433, 2.844799999999009010 ) ;
#5860 = AXIS2_PLACEMENT_3D ( 'NONE', #22195, #13298, #23121 ) ;
#5861 = TOROIDAL_SURFACE ( 'NONE', #14078, 3.606799999999999784, 0.7620000000000000107 ) ;
#5862 = ORIENTED_EDGE ( 'NONE', *, *, #12576, .F. ) ;
#5863 = AXIS2_PLACEMENT_3D ( 'NONE', #1572, #3446, #19157 ) ;
#5864 = DIRECTION ( 'NONE',  ( 0.000000000000000000, -1.000000000000000000, 0.000000000000000000 ) ) ;
#5865 = ORIENTED_EDGE ( 'NONE', *, *, #22712, .T. ) ;
#5866 = LINE ( 'NONE', #789, #2913 ) ;
#5867 = PERSON_AND_ORGANIZATION ( #5446, #1895 ) ;
#5868 = EDGE_CURVE ( 'NONE', #12207, #13662, #12998, .T. ) ;
#5869 = CARTESIAN_POINT ( 'NONE',  ( 15.54479999999999862, -3639.607668064999416, 2279.447335734999797 ) ) ;
#5870 = AXIS2_PLACEMENT_3D ( 'NONE', #15740, #9990, #18895 ) ;
#5871 = ADVANCED_FACE ( 'NONE', ( #15799 ), #3487, .T. ) ;
#5872 = CARTESIAN_POINT ( 'NONE',  ( 17.75414321264302231, -3662.172752710656368, 2245.401715040317413 ) ) ;
#5873 = FACE_OUTER_BOUND ( 'NONE', #20220, .T. ) ;
#5874 = CARTESIAN_POINT ( 'NONE',  ( 10.18227723364999981, -3578.160723028000120, 2257.881333495000035 ) ) ;
#5875 = CARTESIAN_POINT ( 'NONE',  ( 142.4398810773762136, -3578.715266063343279, 2250.236799993183013 ) ) ;
#5876 = EDGE_CURVE ( 'NONE', #21098, #4940, #3635, .T. ) ;
#5877 = ORIENTED_EDGE ( 'NONE', *, *, #20733, .T. ) ;
#5878 = CIRCLE ( 'NONE', #3232, 0.7619999999999987894 ) ;
#5879 = ORIENTED_EDGE ( 'NONE', *, *, #16835, .T. ) ;
#5880 = CARTESIAN_POINT ( 'NONE',  ( 12.69999999997359019, -3596.805099999930007, 2296.210799999999836 ) ) ;
#5881 = ORIENTED_EDGE ( 'NONE', *, *, #4965, .T. ) ;
#5882 = CARTESIAN_POINT ( 'NONE',  ( 139.6999999999999886, -3579.494999999999891, 2239.391000000000076 ) ) ;
#5883 = CIRCLE ( 'NONE', #3617, 0.7619999999999294005 ) ;
#5884 = CARTESIAN_POINT ( 'NONE',  ( 141.9722846325389867, -3661.255981623820844, 2257.824198832787260 ) ) ;
#5885 = ADVANCED_FACE ( 'NONE', ( #14281 ), #6276, .T. ) ;
#5886 = ADVANCED_FACE ( 'NONE', ( #14047 ), #14396, .F. ) ;
#5887 = ORIENTED_EDGE ( 'NONE', *, *, #15425, .F. ) ;
#5888 = DIRECTION ( 'NONE',  ( -1.000000000000000000, 0.000000000000000000, 0.000000000000000000 ) ) ;
#5889 = CARTESIAN_POINT ( 'NONE',  ( 15.50028889993228987, -3658.999884688285874, 2249.998575292800069 ) ) ;
#5890 = VERTEX_POINT ( 'NONE', #12515 ) ;
#5891 = DIRECTION ( 'NONE',  ( 0.000000000000000000, 0.000000000000000000, 1.000000000000000000 ) ) ;
#5892 = CARTESIAN_POINT ( 'NONE',  ( 13.53605320222184893, -3576.775764562235054, 2249.328209726781552 ) ) ;
#5893 = PLANE ( 'NONE',  #2008 ) ;
#5894 = ORIENTED_EDGE ( 'NONE', *, *, #898, .T. ) ;
#5895 = AXIS2_PLACEMENT_3D ( 'NONE', #20871, #1289, #19696 ) ;
#5896 = CYLINDRICAL_SURFACE ( 'NONE', #6272, 2.844800000000001550 ) ;
#5897 = PERSON_AND_ORGANIZATION ( #5446, #1895 ) ;
#5898 = AXIS2_PLACEMENT_3D ( 'NONE', #20895, #22861, #1661 ) ;
#5899 = CARTESIAN_POINT ( 'NONE',  ( 9.855200508358999301, -3659.504986005999854, 2257.962940201000038 ) ) ;
#5900 = CARTESIAN_POINT ( 'NONE',  ( 3.048000000000000043, -3543.299999999999727, 2238.248000000000047 ) ) ;
#5901 = DIRECTION ( 'NONE',  ( -2.356218894535439317E-14, 0.000000000000000000, -1.000000000000000000 ) ) ;
#5902 = CIRCLE ( 'NONE', #13359, 2.844800000000001550 ) ;
#5903 = ORIENTED_EDGE ( 'NONE', *, *, #81, .T. ) ;
#5904 = CARTESIAN_POINT ( 'NONE',  ( 140.9027360924337131, -3662.083407271924443, 2249.469647930371593 ) ) ;
#5905 = ORIENTED_EDGE ( 'NONE', *, *, #11492, .F. ) ;
#5906 = VERTEX_POINT ( 'NONE', #5255 ) ;
#5907 = ORIENTED_EDGE ( 'NONE', *, *, #939, .F. ) ;
#5908 = AXIS2_PLACEMENT_3D ( 'NONE', #17838, #1786, #8934 ) ;
#5909 = DIRECTION ( 'NONE',  ( 0.000000000000000000, 0.000000000000000000, -1.000000000000000000 ) ) ;
#5910 = ORIENTED_EDGE ( 'NONE', *, *, #22158, .T. ) ;
#5911 = CARTESIAN_POINT ( 'NONE',  ( 10.36831320285999958, -3660.851200000000063, 2242.820000000000164 ) ) ;
#5912 = ITEM_DEFINED_TRANSFORMATION ( 'NONE', 'NONE', #6009,  #5611 ) ;
#5913 = CARTESIAN_POINT ( 'NONE',  ( 114.2999999999999972, -3594.099999999999909, 2261.869999999999891 ) ) ;
#5914 = ORIENTED_EDGE ( 'NONE', *, *, #20169, .T. ) ;
#5915 = AXIS2_PLACEMENT_3D ( 'NONE', #4181, #2091, #7818 ) ;
#5916 = CARTESIAN_POINT ( 'NONE',  ( 7.053810164393185644, -3658.615721339214815, 2244.986590707419509 ) ) ;
#5917 = VECTOR ( 'NONE', #7182, 1000.000000000000114 ) ;
#5918 = FACE_BOUND ( 'NONE', #18357, .T. ) ;
#5919 = CARTESIAN_POINT ( 'NONE',  ( 6.997747388991874651, -3579.940010871207051, 2244.748233079088095 ) ) ;
#5920 = LINE ( 'NONE', #1814, #8882 ) ;
#5921 = CALENDAR_DATE ( 2026, 26, 10 ) ;
#5922 = CARTESIAN_POINT ( 'NONE',  ( 12.69999999994000106, -3636.810100000000148, 2292.781800000000203 ) ) ;
#5923 = EDGE_LOOP ( 'NONE', ( #18249, #13158 ) ) ;
#5924 = APPLIED_PERSON_AND_ORGANIZATION_ASSIGNMENT ( #13137, #22149, ( #7485 ) ) ;
#5925 = CARTESIAN_POINT ( 'NONE',  ( 142.4123320799332362, -3658.645882986786091, 2249.813345329157983 ) ) ;
#5926 = VECTOR ( 'NONE', #12741, 1000.000000000000000 ) ;
#5927 = DIRECTION ( 'NONE',  ( -1.000000000000000000, 0.000000000000000000, 0.000000000000000000 ) ) ;
#5928 = ORIENTED_EDGE ( 'NONE', *, *, #13887, .F. ) ;
#5929 = DIRECTION ( 'NONE',  ( 0.000000000000000000, 1.000000000000000000, 0.000000000000000000 ) ) ;
#5930 = TOROIDAL_SURFACE ( 'NONE', #8161, 1.905000000000000027, 1.270000000000000018 ) ;
#5931 = EDGE_CURVE ( 'NONE', #18295, #4608, #218, .T. ) ;
#5932 = EDGE_CURVE ( 'NONE', #6015, #11279, #22342, .T. ) ;
#5933 = CARTESIAN_POINT ( 'NONE',  ( 17.31138602737999932, -3662.880847139000252, 2246.630000000000109 ) ) ;
#5934 = CARTESIAN_POINT ( 'NONE',  ( 85.29320000000001301, -3594.099999999999909, 2239.009999999999764 ) ) ;
#5935 = CARTESIAN_POINT ( 'NONE',  ( 142.5262129393911152, -3579.870018574420101, 2257.957971591534715 ) ) ;
#5936 = EDGE_CURVE ( 'NONE', #18291, #5789, #19787, .T. ) ;
#5937 = CARTESIAN_POINT ( 'NONE',  ( 0.000000000000000000, -3694.430000000000291, 2240.279999999999745 ) ) ;
#5938 = ORIENTED_EDGE ( 'NONE', *, *, #55, .T. ) ;
#5939 = DIRECTION ( 'NONE',  ( 1.000000000000000000, 0.000000000000000000, 0.000000000000000000 ) ) ;
#5940 = CYLINDRICAL_SURFACE ( 'NONE', #184, 0.3809999999999260090 ) ;
#5941 = CARTESIAN_POINT ( 'NONE',  ( 9.394261469291061317, -3543.299999999916054, 2281.667430734604750 ) ) ;
#5942 = CIRCLE ( 'NONE', #18220, 1.269999999999882334 ) ;
#5943 = DIRECTION ( 'NONE',  ( 0.000000000000000000, 0.000000000000000000, -1.000000000000000000 ) ) ;
#5944 = CARTESIAN_POINT ( 'NONE',  ( 142.4830070222579366, -3543.485052020446346, 2255.165585415843907 ) ) ;
#5945 = EDGE_CURVE ( 'NONE', #14242, #16552, #4776, .T. ) ;
#5946 = CARTESIAN_POINT ( 'NONE',  ( 20.32000000000000028, -3568.700000000000273, 2286.368300000000090 ) ) ;
#5947 = CARTESIAN_POINT ( 'NONE',  ( -6.349999999999999645, -3665.601000000000113, 2247.392000000000280 ) ) ;
#5948 = ORIENTED_EDGE ( 'NONE', *, *, #10431, .F. ) ;
#5949 = SECURITY_CLASSIFICATION_LEVEL ( 'unclassified' ) ;
#5950 = DIRECTION ( 'NONE',  ( -1.000000000000000000, 0.000000000000000000, 0.000000000000000000 ) ) ;
#5951 = CARTESIAN_POINT ( 'NONE',  ( 127.0000000000000000, -3619.500000000000000, 2261.869999999999891 ) ) ;
#5952 = LINE ( 'NONE', #20351, #14992 ) ;
#5953 = ORIENTED_EDGE ( 'NONE', *, *, #9138, .T. ) ;
#5954 = CARTESIAN_POINT ( 'NONE',  ( 151.4000000000000057, -3543.329032635400836, 2259.329999999999927 ) ) ;
#5955 = EDGE_CURVE ( 'NONE', #14185, #16978, #9272, .T. ) ;
#5956 = ORIENTED_EDGE ( 'NONE', *, *, #17010, .T. ) ;
#5957 = LINE ( 'NONE', #20570, #12148 ) ;
#5958 = ORIENTED_EDGE ( 'NONE', *, *, #12746, .F. ) ;
#5959 = EDGE_CURVE ( 'NONE', #7862, #4904, #15920, .T. ) ;
#5960 = DIRECTION ( 'NONE',  ( 0.000000000000000000, 0.000000000000000000, -1.000000000000000000 ) ) ;
#5961 = ADVANCED_FACE ( 'NONE', ( #5612 ), #15255, .T. ) ;
#5962 = DIRECTION ( 'NONE',  ( 0.7249994335945011414, 0.000000000000000000, -0.6887494619146010688 ) ) ;
#5963 = ORIENTED_EDGE ( 'NONE', *, *, #7169, .T. ) ;
#5964 = CARTESIAN_POINT ( 'NONE',  ( 15.41268679713999923, -3601.063670452999759, 2296.591799999999694 ) ) ;
#5965 = CYLINDRICAL_SURFACE ( 'NONE', #9552, 0.3809999999998115450 ) ;
#5966 = ORIENTED_EDGE ( 'NONE', *, *, #8742, .F. ) ;
#5967 = DIRECTION ( 'NONE',  ( -1.000000000000000000, 0.000000000000000000, 0.000000000000000000 ) ) ;
#5968 = CYLINDRICAL_SURFACE ( 'NONE', #21063, 0.7619999999999294005 ) ;
#5969 = ORIENTED_EDGE ( 'NONE', *, *, #5216, .F. ) ;
#5970 = AXIS2_PLACEMENT_3D ( 'NONE', #22322, #18693, #15422 ) ;
#5971 = CARTESIAN_POINT ( 'NONE',  ( 137.3683132029851208, -3580.841200000048957, 2239.391000000000076 ) ) ;
#5972 = PRODUCT_DEFINITION_CONTEXT ( 'detailed design', #1674, 'design' ) ;
#5973 = EDGE_CURVE ( 'NONE', #1122, #3687, #20482, .T. ) ;
#5974 = EDGE_LOOP ( 'NONE', ( #21258, #19490, #21220, #839 ) ) ;
#5975 = AXIS2_PLACEMENT_3D ( 'NONE', #15322, #1013, #8288 ) ;
#5976 = CARTESIAN_POINT ( 'NONE',  ( 145.1262588623648639, -3581.288617102159606, 2245.910525606668671 ) ) ;
#5977 = CALENDAR_DATE ( 2026, 26, 10 ) ;
#5978 = DIRECTION ( 'NONE',  ( -1.000000000000000000, 0.000000000000000000, 0.000000000000000000 ) ) ;
#5979 = CARTESIAN_POINT ( 'NONE',  ( 12.69999999999999929, -3579.494999999999891, 2272.030000000000200 ) ) ;
#5980 = EDGE_CURVE ( 'NONE', #444, #20696, #14512, .T. ) ;
#5981 = CARTESIAN_POINT ( 'NONE',  ( 142.2033847376006861, -3578.142761313953997, 2250.145277428746340 ) ) ;
#5982 = EDGE_LOOP ( 'NONE', ( #16663, #13524, #860, #21265, #8953, #12464, #21427 ) ) ;
#5983 = VECTOR ( 'NONE', #9600, 1000.000000000000000 ) ;
#5984 = ORIENTED_EDGE ( 'NONE', *, *, #3127, .F. ) ;
#5985 = DIRECTION ( 'NONE',  ( 1.000000000000000000, 0.000000000000000000, 0.000000000000000000 ) ) ;
#5986 = ORIENTED_EDGE ( 'NONE', *, *, #9253, .T. ) ;
#5987 = APPLIED_SECURITY_CLASSIFICATION_ASSIGNMENT ( #17188, ( #10138 ) ) ;
#5988 = CARTESIAN_POINT ( 'NONE',  ( 12.70000000000000462, -3596.652698770568804, 2279.817639764978139 ) ) ;
#5989 = VECTOR ( 'NONE', #1217, 1000.000000000000000 ) ;
#5990 = CARTESIAN_POINT ( 'NONE',  ( 15.55031652512126250, -3543.399485434554663, 2254.996725890375274 ) ) ;
#5991 = EDGE_CURVE ( 'NONE', #6867, #3180, #10524, .T. ) ;
#5992 = EDGE_CURVE ( 'NONE', #3669, #11744, #20130, .T. ) ;
#5993 = ORIENTED_EDGE ( 'NONE', *, *, #6250, .T. ) ;
#5994 = CARTESIAN_POINT ( 'NONE',  ( 20.09942059832000183, -3544.570000000000164, 2260.390449568000349 ) ) ;
#5995 = ORIENTED_EDGE ( 'NONE', *, *, #15180, .F. ) ;
#5996 = CARTESIAN_POINT ( 'NONE',  ( -8.890000000032001637, -3577.513800000000174, 2245.060313203000078 ) ) ;
#5997 = CARTESIAN_POINT ( 'NONE',  ( 13.55725822396861524, -3576.782357048964968, 2249.335288272477101 ) ) ;
#5998 = CARTESIAN_POINT ( 'NONE',  ( 142.2474702748325512, -3580.761556601727989, 2249.508564178021970 ) ) ;
#5999 = EDGE_CURVE ( 'NONE', #12999, #5355, #10005, .T. ) ;
#6000 = ORIENTED_EDGE ( 'NONE', *, *, #20824, .F. ) ;
#6001 = CARTESIAN_POINT ( 'NONE',  ( 20.32000000000000028, -3662.045000000000073, 2247.392000000000280 ) ) ;
#6002 = CALENDAR_DATE ( 2026, 26, 10 ) ;
#6003 = CIRCLE ( 'NONE', #13461, 0.7619999999999683693 ) ;
#6004 = CARTESIAN_POINT ( 'NONE',  ( 60.21459350832999746, -3543.299999999999727, 2280.170699136999701 ) ) ;
#6005 = DIRECTION ( 'NONE',  ( 0.000000000000000000, 0.000000000000000000, 1.000000000000000000 ) ) ;
#6006 = EDGE_LOOP ( 'NONE', ( #19604, #21145, #7257, #9959 ) ) ;
#6007 = APPLIED_APPROVAL_ASSIGNMENT ( #10348, ( #2608 ) ) ;
#6008 = CARTESIAN_POINT ( 'NONE',  ( 20.75864668056231821, -3543.309784082139231, 2259.501798909290756 ) ) ;
#6009 = AXIS2_PLACEMENT_3D ( 'NONE', #15472, #18637, #18744 ) ;
#6010 = ADVANCED_FACE ( 'NONE', ( #4299 ), #6068, .T. ) ;
#6011 = LINE ( 'NONE', #11272, #17306 ) ;
#6012 = EDGE_CURVE ( 'NONE', #7575, #22920, #22100, .T. ) ;
#6013 = ORIENTED_EDGE ( 'NONE', *, *, #2662, .T. ) ;
#6014 = CARTESIAN_POINT ( 'NONE',  ( 141.8956724088833994, -3661.315849440774400, 2249.983377711600951 ) ) ;
#6015 = VERTEX_POINT ( 'NONE', #5954 ) ;
#6016 = EDGE_LOOP ( 'NONE', ( #2066, #22665 ) ) ;
#6017 = AXIS2_PLACEMENT_3D ( 'NONE', #8186, #16963, #12045 ) ;
#6018 = EDGE_CURVE ( 'NONE', #2427, #15790, #4391, .T. ) ;
#6019 = LINE ( 'NONE', #8001, #6938 ) ;
#6020 = ORIENTED_EDGE ( 'NONE', *, *, #13208, .T. ) ;
#6021 = SECURITY_CLASSIFICATION ( '', '', #13689 ) ;
#6022 = CARTESIAN_POINT ( 'NONE',  ( -6.349999999999999645, -3578.860000000000127, 2247.392000000000280 ) ) ;
#6023 = CARTESIAN_POINT ( 'NONE',  ( 38.10000000000000142, -3644.899999999999636, 2239.009999999999764 ) ) ;
#6024 = APPROVAL_PERSON_ORGANIZATION ( #1787, #3045, #10919 ) ;
#6025 = ORIENTED_EDGE ( 'NONE', *, *, #13883, .T. ) ;
#6026 = CARTESIAN_POINT ( 'NONE',  ( 7.275104262493744756, -3657.707260169260735, 2245.917323013845817 ) ) ;
#6027 =( NAMED_UNIT ( * ) PLANE_ANGLE_UNIT ( ) SI_UNIT ( $, .RADIAN. ) );
#6028 = FACE_OUTER_BOUND ( 'NONE', #11655, .T. ) ;
#6029 = ADVANCED_BREP_SHAPE_REPRESENTATION ( '', ( #21083, #5611 ), #4481 ) ;
#6030 = CYLINDRICAL_SURFACE ( 'NONE', #5510, 0.3809999999998115450 ) ;
#6031 = PERSON_AND_ORGANIZATION ( #5446, #1895 ) ;
#6032 = CARTESIAN_POINT ( 'NONE',  ( 95.25000000000000000, -3694.430000000000291, 2247.392000000000280 ) ) ;
#6033 = DIRECTION ( 'NONE',  ( 0.000000000000000000, 0.000000000000000000, 1.000000000000000000 ) ) ;
#6034 = CYLINDRICAL_SURFACE ( 'NONE', #7052, 0.7620000000000000107 ) ;
#6035 = AXIS2_PLACEMENT_3D ( 'NONE', #17156, #6863, #6745 ) ;
#6036 = LOCAL_TIME ( 17, 37, 43.00000000000000000, #12602 ) ;
#6037 = EDGE_LOOP ( 'NONE', ( #2031, #4368, #6948, #5005 ) ) ;
#6038 = DIRECTION ( 'NONE',  ( -0.8660254037816071948, 0.5000000000049040771, 0.000000000000000000 ) ) ;
#6039 = CYLINDRICAL_SURFACE ( 'NONE', #11403, 0.7619999999999294005 ) ;
#6040 = ORIENTED_EDGE ( 'NONE', *, *, #3183, .F. ) ;
#6041 = AXIS2_PLACEMENT_3D ( 'NONE', #18352, #761, #996 ) ;
#6042 = CARTESIAN_POINT ( 'NONE',  ( 110.6932000000009992, -3594.099999999999909, 2260.600000000000364 ) ) ;
#6043 = ORIENTED_EDGE ( 'NONE', *, *, #2007, .T. ) ;
#6044 = VECTOR ( 'NONE', #4282, 1000.000000000000000 ) ;
#6045 = CARTESIAN_POINT ( 'NONE',  ( 139.6999999999999886, -3570.287499999999909, 2279.817639999999756 ) ) ;
#6046 = ORIENTED_EDGE ( 'NONE', *, *, #18867, .F. ) ;
#6047 = EDGE_LOOP ( 'NONE', ( #20542, #18726 ) ) ;
#6048 = B_SPLINE_CURVE_WITH_KNOTS ( 'NONE', 3,
 ( #7059, #5411, #14664, #20055 ),
 .UNSPECIFIED., .F., .F.,
 ( 4, 4 ),
 ( 0.000000000000000000, 1.000000000000000000 ),
 .UNSPECIFIED. ) ;
#6049 = CYLINDRICAL_SURFACE ( 'NONE', #16864, 1.269999999999898099 ) ;
#6050 = CARTESIAN_POINT ( 'NONE',  ( 12.69999999976711180, -3582.627340905157780, 2239.009999999999764 ) ) ;
#6051 = B_SPLINE_CURVE_WITH_KNOTS ( 'NONE', 3,
 ( #6557, #10051, #12047, #17081, #6678, #11814, #19203, #6786, #13816, #13927, #13457, #4544, #3140, #22584, #11687, #18844, #21077, #8074, #2788 ),
 .UNSPECIFIED., .F., .F.,
 ( 4, 1, 1, 1, 1, 1, 1, 1, 1, 1, 1, 1, 1, 1, 1, 1, 4 ),
 ( 0.000000000000000000, 0.06250000000000000000, 0.1250000000000000000, 0.1875000000000000000, 0.2500000000000000000, 0.3125000000000000000, 0.3750000000000000000, 0.4375000000000000000, 0.5000000000000000000, 0.5625000000000000000, 0.6250000000000000000, 0.6875000000000000000, 0.7500000000000000000, 0.8125000000000000000, 0.8750000000000000000, 0.9375000000000000000, 1.000000000000000000 ),
 .UNSPECIFIED. ) ;
#6052 = CARTESIAN_POINT ( 'NONE',  ( 10.92596159350999940, -3601.729223875000116, 2279.676121195000178 ) ) ;
#6053 = APPROVAL ( #22578, 'UNKNOWN' ) ;
#6054 = CARTESIAN_POINT ( 'NONE',  ( 151.4000000000000057, -3694.938000000000102, 2295.829799999999977 ) ) ;
#6055 = DIRECTION ( 'NONE',  ( 0.000000000000000000, -1.000000000000000000, 0.000000000000000000 ) ) ;
#6056 = DIRECTION ( 'NONE',  ( 1.000000000000000000, 0.000000000000000000, 0.000000000000000000 ) ) ;
#6057 = LOCAL_TIME ( 17, 37, 43.00000000000000000, #6337 ) ;
#6058 = CARTESIAN_POINT ( 'NONE',  ( 16.19063073453000001, -3695.699999999999818, 2282.113800000000083 ) ) ;
#6059 = VERTEX_POINT ( 'NONE', #21877 ) ;
#6060 = DATE_AND_TIME ( #21982, #11602 ) ;
#6061 = EDGE_CURVE ( 'NONE', #14108, #4104, #18999, .T. ) ;
#6062 = LINE ( 'NONE', #20348, #15773 ) ;
#6063 = VECTOR ( 'NONE', #403, 1000.000000000000000 ) ;
#6064 = CIRCLE ( 'NONE', #19147, 3.606799999998994366 ) ;
#6065 = CARTESIAN_POINT ( 'NONE',  ( 16.19063073453000001, -3695.699999999999818, 2282.113800000000083 ) ) ;
#6066 = DIRECTION ( 'NONE',  ( -0.8660254037821902839, 0.5000000000038942183, 1.814359422184980810E-12 ) ) ;
#6067 = ORIENTED_EDGE ( 'NONE', *, *, #5111, .F. ) ;
#6068 = CYLINDRICAL_SURFACE ( 'NONE', #13016, 3.175000000000149925 ) ;
#6069 = DIRECTION ( 'NONE',  ( 0.000000000000000000, 0.000000000000000000, 1.000000000000000000 ) ) ;
#6070 = EDGE_LOOP ( 'NONE', ( #1222, #21647 ) ) ;
#6071 = DIRECTION ( 'NONE',  ( 1.000000000000000000, 0.000000000000000000, 0.000000000000000000 ) ) ;
#6072 = CARTESIAN_POINT ( 'NONE',  ( 131.7757523116999891, -3695.699999999999818, 2259.837999999999738 ) ) ;
#6073 = DIRECTION ( 'NONE',  ( 1.000000000000000000, 0.000000000000000000, 0.000000000000000000 ) ) ;
#6074 = ORIENTED_EDGE ( 'NONE', *, *, #1037, .F. ) ;
#6075 = CARTESIAN_POINT ( 'NONE',  ( 9.987313202991520811, -3577.928829547366604, 2239.009999999999764 ) ) ;
#6076 = AXIS2_PLACEMENT_3D ( 'NONE', #14626, #2203, #21767 ) ;
#6077 = DIRECTION ( 'NONE',  ( 0.000000000000000000, 0.000000000000000000, 1.000000000000000000 ) ) ;
#6078 = PRODUCT_RELATED_PRODUCT_CATEGORY ( 'detail', '', ( #12762 ) ) ;
#6079 = VECTOR ( 'NONE', #8202, 1000.000000000000000 ) ;
#6080 = ORIENTED_EDGE ( 'NONE', *, *, #11144, .F. ) ;
#6081 = CARTESIAN_POINT ( 'NONE',  ( -6.730999999999999872, -3660.140000000000327, 2247.392000000000280 ) ) ;
#6082 = CARTESIAN_POINT ( 'NONE',  ( 144.3113860274000047, -3662.880847139000252, 2246.630000000000109 ) ) ;
#6083 = ORIENTED_EDGE ( 'NONE', *, *, #9997, .T. ) ;
#6084 = ORIENTED_EDGE ( 'NONE', *, *, #7023, .F. ) ;
#6085 = EDGE_CURVE ( 'NONE', #7043, #7639, #19368, .T. ) ;
#6086 = DIRECTION ( 'NONE',  ( 1.000000000000000000, 0.000000000000000000, 0.000000000000000000 ) ) ;
#6087 = ADVANCED_FACE ( 'NONE', ( #326 ), #20135, .T. ) ;
#6088 = EDGE_LOOP ( 'NONE', ( #20831, #21147, #8209, #4866 ) ) ;
#6089 = CARTESIAN_POINT ( 'NONE',  ( 145.2719119545006947, -3580.765843483391563, 2245.279837210061032 ) ) ;
#6090 =( BOUNDED_CURVE ( )  B_SPLINE_CURVE ( 3, ( #13319, #13092, #15311, #16939 ),
 .UNSPECIFIED., .F., .T. ) 
 B_SPLINE_CURVE_WITH_KNOTS ( ( 4, 4 ),
 ( 1.570796327146205540, 3.141592653589829531 ),
 .UNSPECIFIED. ) 
 CURVE ( )  GEOMETRIC_REPRESENTATION_ITEM ( )  RATIONAL_B_SPLINE_CURVE ( ( 1.000000000000000000, 0.8047378542071605967, 0.8047378542071605967, 1.000000000000000000 ) ) 
 REPRESENTATION_ITEM ( '' )  );
#6091 = DATE_AND_TIME ( #689, #18709 ) ;
#6092 = ADVANCED_FACE ( 'NONE', ( #552 ), #5848, .F. ) ;
#6093 = CARTESIAN_POINT ( 'NONE',  ( 139.6999999999999886, -3582.339799999999286, 2257.592639999999847 ) ) ;
#6094 = FACE_OUTER_BOUND ( 'NONE', #6686, .T. ) ;
#6095 = AXIS2_PLACEMENT_3D ( 'NONE', #13567, #4654, #18379 ) ;
#6096 = AXIS2_PLACEMENT_3D ( 'NONE', #10283, #6673, #19429 ) ;
#6097 = CARTESIAN_POINT ( 'NONE',  ( 50.79999999999999716, -3670.300000000000182, 2239.771999999999935 ) ) ;
#6098 = CARTESIAN_POINT ( 'NONE',  ( 72.59320000000001016, -3670.300000000000182, 2259.837999999999738 ) ) ;
#6099 = CIRCLE ( 'NONE', #1978, 0.7619999999999294005 ) ;
#6100 = CARTESIAN_POINT ( 'NONE',  ( 137.8823296110995216, -3577.304701220188235, 2249.774946555156021 ) ) ;
#6101 = EDGE_LOOP ( 'NONE', ( #13264, #10913, #22715, #2650 ) ) ;
#6102 = DIRECTION ( 'NONE',  ( 0.000000000000000000, 0.000000000000000000, -1.000000000000000000 ) ) ;
#6103 = CARTESIAN_POINT ( 'NONE',  ( 1.270000000000000018, -3544.570000000000164, 2259.329999999999927 ) ) ;
#6104 = EDGE_LOOP ( 'NONE', ( #19733, #8433, #271, #1335 ) ) ;
#6105 = EDGE_CURVE ( 'NONE', #18286, #18510, #17484, .T. ) ;
#6106 = DIRECTION ( 'NONE',  ( 0.000000000000000000, 1.000000000000000000, 0.000000000000000000 ) ) ;
#6107 = DIRECTION ( 'NONE',  ( 0.000000000000000000, 0.000000000000000000, 1.000000000000000000 ) ) ;
#6108 = AXIS2_PLACEMENT_3D ( 'NONE', #20186, #14915, #6127 ) ;
#6109 = ORIENTED_EDGE ( 'NONE', *, *, #4408, .T. ) ;
#6110 = ORIENTED_EDGE ( 'NONE', *, *, #5687, .F. ) ;
#6111 = ORIENTED_EDGE ( 'NONE', *, *, #548, .T. ) ;
#6112 = CARTESIAN_POINT ( 'NONE',  ( 15.03168679714000078, -3598.151299999999992, 2296.210799999999836 ) ) ;
#6113 = AXIS2_PLACEMENT_3D ( 'NONE', #6514, #14954, #20671 ) ;
#6114 = VERTEX_POINT ( 'NONE', #11110 ) ;
#6115 = CIRCLE ( 'NONE', #852, 3.606800000000021100 ) ;
#6116 = CARTESIAN_POINT ( 'NONE',  ( 35.56000000000000227, -3544.570000000000164, 2251.506800000000112 ) ) ;
#6117 = CARTESIAN_POINT ( 'NONE',  ( 12.56749442210865197, -3576.650097218246174, 2249.183428692989310 ) ) ;
#6118 = CARTESIAN_POINT ( 'NONE',  ( 142.5253973193343597, -3579.881039274069281, 2250.055385365074471 ) ) ;
#6119 = VERTEX_POINT ( 'NONE', #7584 ) ;
#6120 = DIRECTION ( 'NONE',  ( -1.000000000000000000, 0.000000000000000000, 0.000000000000000000 ) ) ;
#6121 = APPROVAL_DATE_TIME ( #7521, #11912 ) ;
#6122 = EDGE_CURVE ( 'NONE', #9353, #3735, #21403, .T. ) ;
#6123 = DIRECTION ( 'NONE',  ( -1.000000000000000000, 0.000000000000000000, 0.000000000000000000 ) ) ;
#6124 = CARTESIAN_POINT ( 'NONE',  ( 20.53780452085382180, -3543.526739948642899, 2260.054530369292934 ) ) ;
#6125 = AXIS2_PLACEMENT_3D ( 'NONE', #1525, #21452, #12316 ) ;
#6126 = EDGE_CURVE ( 'NONE', #2858, #16219, #768, .T. ) ;
#6127 = DIRECTION ( 'NONE',  ( 1.000000000000000000, 0.000000000000000000, 0.000000000000000000 ) ) ;
#6128 = ADVANCED_FACE ( 'NONE', ( #22208 ), #6178, .F. ) ;
#6129 = ORIENTED_EDGE ( 'NONE', *, *, #1491, .T. ) ;
#6130 = AXIS2_PLACEMENT_3D ( 'NONE', #18435, #16787, #8233 ) ;
#6131 = CARTESIAN_POINT ( 'NONE',  ( -12.54218463273320339, -3577.513799999517232, 2245.060313203004171 ) ) ;
#6132 = VECTOR ( 'NONE', #22741, 1000.000000000000000 ) ;
#6133 = ORIENTED_EDGE ( 'NONE', *, *, #20896, .T. ) ;
#6134 = ORIENTED_EDGE ( 'NONE', *, *, #1531, .T. ) ;
#6135 = ORIENTED_EDGE ( 'NONE', *, *, #11116, .T. ) ;
#6136 = CARTESIAN_POINT ( 'NONE',  ( 101.5999999999999943, -3619.500000000000000, 2259.837999999999738 ) ) ;
#6137 = CARTESIAN_POINT ( 'NONE',  ( 61.26424768829000556, -3544.061999999999898, 2280.589800000000196 ) ) ;
#6138 = CIRCLE ( 'NONE', #17337, 5.079999999999973426 ) ;
#6139 = ADVANCED_FACE ( 'NONE', ( #12023 ), #10378, .T. ) ;
#6140 = VERTEX_POINT ( 'NONE', #18696 ) ;
#6141 = DIRECTION ( 'NONE',  ( 0.000000000000000000, 1.000000000000000000, 0.000000000000000000 ) ) ;
#6142 = CARTESIAN_POINT ( 'NONE',  ( 151.1299999999999955, -3660.140000000000327, 2243.277199999999993 ) ) ;
#6143 = DIRECTION ( 'NONE',  ( 0.000000000000000000, 0.000000000000000000, 1.000000000000000000 ) ) ;
#6144 = APPROVAL_STATUS ( 'not_yet_approved' ) ;
#6145 = DIRECTION ( 'NONE',  ( 0.000000000000000000, 0.000000000000000000, 1.000000000000000000 ) ) ;
#6146 = CYLINDRICAL_SURFACE ( 'NONE', #18074, 2.844799999999999773 ) ;
#6147 = ADVANCED_FACE ( 'NONE', ( #1234 ), #13545, .F. ) ;
#6148 = DIRECTION ( 'NONE',  ( 1.000000000000000000, 0.000000000000000000, -1.224646799147353207E-16 ) ) ;
#6149 = ORIENTED_EDGE ( 'NONE', *, *, #5401, .T. ) ;
#6150 = B_SPLINE_CURVE_WITH_KNOTS ( 'NONE', 3,
 ( #919, #9719, #11940, #22136 ),
 .UNSPECIFIED., .F., .F.,
 ( 4, 4 ),
 ( 0.000000000000000000, 1.000000000000000000 ),
 .UNSPECIFIED. ) ;
#6151 = LINE ( 'NONE', #15055, #11108 ) ;
#6152 = VECTOR ( 'NONE', #8403, 1000.000000000000000 ) ;
#6153 = FACE_OUTER_BOUND ( 'NONE', #11040, .T. ) ;
#6154 = EDGE_LOOP ( 'NONE', ( #1302, #1209, #8297, #15186 ) ) ;
#6155 = LINE ( 'NONE', #14943, #22991 ) ;
#6156 = FACE_OUTER_BOUND ( 'NONE', #1500, .T. ) ;
#6157 = ORIENTED_EDGE ( 'NONE', *, *, #18020, .T. ) ;
#6158 = ORIENTED_EDGE ( 'NONE', *, *, #1813, .F. ) ;
#6159 = LINE ( 'NONE', #2739, #19136 ) ;
#6160 = DIRECTION ( 'NONE',  ( -2.318894227180156550E-14, -1.000000000000000000, 0.000000000000000000 ) ) ;
#6161 = EDGE_CURVE ( 'NONE', #12197, #6431, #18942, .T. ) ;
#6162 = CARTESIAN_POINT ( 'NONE',  ( 11.47192027633000144, -3602.070229274999747, 2279.750852048000070 ) ) ;
#6163 = EDGE_CURVE ( 'NONE', #3849, #5628, #8094, .T. ) ;
#6164 = CARTESIAN_POINT ( 'NONE',  ( 151.6380000000000052, -3543.299999999999727, 2295.829799999999977 ) ) ;
#6165 = CARTESIAN_POINT ( 'NONE',  ( 139.6999999999999886, -3654.043999999999869, 2239.391000000000076 ) ) ;
#6166 = DIRECTION ( 'NONE',  ( -1.224646799147353207E-16, 1.000000000000000000, 0.000000000000000000 ) ) ;
#6167 = AXIS2_PLACEMENT_3D ( 'NONE', #9903, #6411, #20687 ) ;
#6168 = FACE_OUTER_BOUND ( 'NONE', #20243, .T. ) ;
#6169 = ORIENTED_EDGE ( 'NONE', *, *, #7501, .F. ) ;
#6170 = APPROVAL_STATUS ( 'not_yet_approved' ) ;
#6171 = AXIS2_PLACEMENT_3D ( 'NONE', #21860, #14374, #21405 ) ;
#6172 = VERTEX_POINT ( 'NONE', #8275 ) ;
#6173 = AXIS2_PLACEMENT_3D ( 'NONE', #22535, #6630, #17267 ) ;
#6174 = CARTESIAN_POINT ( 'NONE',  ( 145.0244890045273962, -3657.428455897194453, 2246.524599549557479 ) ) ;
#6175 = CARTESIAN_POINT ( 'NONE',  ( 63.50000000000000000, -3644.899999999999636, 2239.009999999999764 ) ) ;
#6176 = DIRECTION ( 'NONE',  ( -3.028227728787145447E-14, -0.5000000000043240966, -0.8660254037819421491 ) ) ;
#6177 = EDGE_LOOP ( 'NONE', ( #1631, #8717, #15513, #19488 ) ) ;
#6178 = CYLINDRICAL_SURFACE ( 'NONE', #9629, 6.349999999999855760 ) ;
#6179 = ORIENTED_EDGE ( 'NONE', *, *, #13727, .T. ) ;
#6180 = CIRCLE ( 'NONE', #5494, 3.606799999999993567 ) ;
#6181 = FACE_BOUND ( 'NONE', #1047, .T. ) ;
#6182 = CARTESIAN_POINT ( 'NONE',  ( 134.0203227398999957, -3578.860230781999689, 2244.548186305999934 ) ) ;
#6183 = VERTEX_POINT ( 'NONE', #15195 ) ;
#6184 = CARTESIAN_POINT ( 'NONE',  ( 130.6067999999989979, -3619.500000000000000, 2260.600000000000364 ) ) ;
#6185 = AXIS2_PLACEMENT_3D ( 'NONE', #4157, #6708, #13172 ) ;
#6186 = FACE_OUTER_BOUND ( 'NONE', #16742, .T. ) ;
#6187 = CIRCLE ( 'NONE', #19646, 5.460999999999938126 ) ;
#6188 = DIRECTION ( 'NONE',  ( 0.000000000000000000, 0.000000000000000000, -1.000000000000000000 ) ) ;
#6189 = CIRCLE ( 'NONE', #5459, 0.7619999999999294005 ) ;
#6190 = ORIENTED_EDGE ( 'NONE', *, *, #5406, .T. ) ;
#6191 = DIRECTION ( 'NONE',  ( -1.000000000000000000, 0.000000000000000000, 0.000000000000000000 ) ) ;
#6192 = CARTESIAN_POINT ( 'NONE',  ( 14.71622495092000094, -3637.486870620999980, 2279.634028774999933 ) ) ;
#6193 = CARTESIAN_POINT ( 'NONE',  ( 3.810000000000000053, -3544.061999999999898, 2238.248000000000047 ) ) ;
#6194 = CARTESIAN_POINT ( 'NONE',  ( 130.6067999999989979, -3568.700000000000273, 2260.600000000000364 ) ) ;
#6195 = ORIENTED_EDGE ( 'NONE', *, *, #16299, .F. ) ;
#6196 = CARTESIAN_POINT ( 'NONE',  ( 138.3436566013999993, -3581.844255679000071, 2239.391000000000076 ) ) ;
#6197 = AXIS2_PLACEMENT_3D ( 'NONE', #10821, #7312, #14921 ) ;
#6198 = ORIENTED_EDGE ( 'NONE', *, *, #11868, .F. ) ;
#6199 = CARTESIAN_POINT ( 'NONE',  ( 145.0128742528999908, -3581.600847139000052, 2246.630000000000109 ) ) ;
#6200 = AXIS2_PLACEMENT_3D ( 'NONE', #10905, #7742, #15001 ) ;
#6201 = DATE_TIME_ROLE ( 'classification_date' ) ;
#6202 = AXIS2_PLACEMENT_3D ( 'NONE', #226, #5853, #9354 ) ;
#6203 = FACE_OUTER_BOUND ( 'NONE', #949, .T. ) ;
#6204 = CARTESIAN_POINT ( 'NONE',  ( 17.98800820957344726, -3661.672316069987119, 2244.994777904991679 ) ) ;
#6205 = TOROIDAL_SURFACE ( 'NONE', #18924, 3.606799999999999784, 0.7620000000000000107 ) ;
#6206 = LINE ( 'NONE', #13345, #3995 ) ;
#6207 = APPLIED_PERSON_AND_ORGANIZATION_ASSIGNMENT ( #270, #822, ( #9636 ) ) ;
#6208 = CARTESIAN_POINT ( 'NONE',  ( 142.0316867971268096, -3580.841200000091249, 2239.391000000000076 ) ) ;
#6209 = MANIFOLD_SOLID_BREP ( 'SOLID45-10[1]', #19962 ) ;
#6210 = FACE_OUTER_BOUND ( 'NONE', #10819, .T. ) ;
#6211 = ORIENTED_EDGE ( 'NONE', *, *, #22539, .F. ) ;
#6212 = DIRECTION ( 'NONE',  ( -1.000000000000000000, 0.000000000000000000, 0.000000000000000000 ) ) ;
#6213 = ADVANCED_FACE ( 'NONE', ( #11546 ), #18814, .F. ) ;
#6214 = CARTESIAN_POINT ( 'NONE',  ( 98.75520000000000209, -3568.700000000000273, 2261.869999999999891 ) ) ;
#6215 = ORIENTED_EDGE ( 'NONE', *, *, #4987, .F. ) ;
#6216 = EDGE_CURVE ( 'NONE', #22780, #3143, #20466, .T. ) ;
#6217 = VECTOR ( 'NONE', #19417, 1000.000000000000114 ) ;
#6218 = DIRECTION ( 'NONE',  ( 0.000000000000000000, -0.8660254037825031448, -0.5000000000033524294 ) ) ;
#6219 = CARTESIAN_POINT ( 'NONE',  ( 15.38584772739802986, -3543.678681369468450, 2255.408757311840873 ) ) ;
#6220 = CIRCLE ( 'NONE', #9213, 2.844800000000091700 ) ;
#6221 = EDGE_CURVE ( 'NONE', #6713, #15342, #12203, .T. ) ;
#6222 = ORIENTED_EDGE ( 'NONE', *, *, #6378, .T. ) ;
#6223 = VECTOR ( 'NONE', #10871, 1000.000000000000000 ) ;
#6224 = VERTEX_POINT ( 'NONE', #8043 ) ;
#6225 = ORIENTED_EDGE ( 'NONE', *, *, #2631, .T. ) ;
#6226 = DIRECTION ( 'NONE',  ( 0.000000000000000000, 0.000000000000000000, 1.000000000000000000 ) ) ;
#6227 =( BOUNDED_CURVE ( )  B_SPLINE_CURVE ( 3, ( #6387, #20658, #11193, #11995 ),
 .UNSPECIFIED., .F., .F. ) 
 B_SPLINE_CURVE_WITH_KNOTS ( ( 4, 4 ),
 ( 4.620504083482610562E-16, 1.570796326139804799 ),
 .UNSPECIFIED. ) 
 CURVE ( )  GEOMETRIC_REPRESENTATION_ITEM ( )  RATIONAL_B_SPLINE_CURVE ( ( 1.000000000000000000, 0.8047378542787717581, 0.8047378542787717581, 1.000000000000000000 ) ) 
 REPRESENTATION_ITEM ( '' )  );
#6228 = ORIENTED_EDGE ( 'NONE', *, *, #22096, .T. ) ;
#6229 = DIRECTION ( 'NONE',  ( -1.000000000000000000, 0.000000000000000000, 0.000000000000000000 ) ) ;
#6230 = CARTESIAN_POINT ( 'NONE',  ( 14.93501350881909850, -3577.734074929383951, 2250.004932963394367 ) ) ;
#6231 = DIRECTION ( 'NONE',  ( 1.000000000000000000, 0.000000000000000000, 0.000000000000000000 ) ) ;
#6232 = AXIS2_PLACEMENT_3D ( 'NONE', #19337, #10187, #8670 ) ;
#6233 = EDGE_CURVE ( 'NONE', #14640, #15062, #8466, .T. ) ;
#6234 = CARTESIAN_POINT ( 'NONE',  ( 141.9421027588409174, -3581.246006357328497, 2248.941170909273296 ) ) ;
#6235 = VERTEX_POINT ( 'NONE', #22325 ) ;
#6236 = DIRECTION ( 'NONE',  ( 0.000000000000000000, 0.000000000000000000, -1.000000000000000000 ) ) ;
#6237 = PERSON_AND_ORGANIZATION_ROLE ( 'design_supplier' ) ;
#6238 = DIRECTION ( 'NONE',  ( 0.000000000000000000, 0.000000000000000000, -1.000000000000000000 ) ) ;
#6239 = DIRECTION ( 'NONE',  ( 1.000000000000000000, 0.000000000000000000, 0.000000000000000000 ) ) ;
#6240 = ADVANCED_FACE ( 'NONE', ( #19173 ), #15571, .T. ) ;
#6241 = PRODUCT_DEFINITION_SHAPE ( 'NONE', 'NONE',  #23171 ) ;
#6242 = CARTESIAN_POINT ( 'NONE',  ( 139.6999999999999886, -3576.650200000000950, 2257.592639999999847 ) ) ;
#6243 = AXIS2_PLACEMENT_3D ( 'NONE', #6329, #13701, #18728 ) ;
#6244 = ORIENTED_EDGE ( 'NONE', *, *, #14237, .F. ) ;
#6245 = DIRECTION ( 'NONE',  ( 0.000000000000000000, 1.000000000000000000, 0.000000000000000000 ) ) ;
#6246 = AXIS2_PLACEMENT_3D ( 'NONE', #6765, #12027, #10615 ) ;
#6247 = EDGE_LOOP ( 'NONE', ( #15121, #19869 ) ) ;
#6248 = ORIENTED_EDGE ( 'NONE', *, *, #3343, .T. ) ;
#6249 = VERTEX_POINT ( 'NONE', #6407 ) ;
#6250 = EDGE_CURVE ( 'NONE', #11029, #4616, #4413, .T. ) ;
#6251 = EDGE_CURVE ( 'NONE', #9808, #8713, #4344, .T. ) ;
#6252 = FACE_OUTER_BOUND ( 'NONE', #21703, .T. ) ;
#6253 = MANIFOLD_SOLID_BREP ( 'TORNILLO[1]', #6493 ) ;
#6254 = VERTEX_POINT ( 'NONE', #2885 ) ;
#6255 = CARTESIAN_POINT ( 'NONE',  ( 9.987313202835000681, -3597.931329547144287, 2296.591799999999694 ) ) ;
#6256 = FACE_OUTER_BOUND ( 'NONE', #18103, .T. ) ;
#6257 = EDGE_LOOP ( 'NONE', ( #11586, #13019, #16815, #22480 ) ) ;
#6258 = DIRECTION ( 'NONE',  ( 0.000000000000000000, -1.000000000000000000, 0.000000000000000000 ) ) ;
#6259 =( NAMED_UNIT ( * ) SI_UNIT ( $, .STERADIAN. ) SOLID_ANGLE_UNIT ( ) );
#6260 = CARTESIAN_POINT ( 'NONE',  ( 9.987313202833000503, -3599.497499999999945, 2296.210799999999836 ) ) ;
#6261 = AXIS2_PLACEMENT_3D ( 'NONE', #22127, #7494, #2340 ) ;
#6262 = DIRECTION ( 'NONE',  ( 0.000000000000000000, 2.336881798971000105E-14, 1.000000000000000000 ) ) ;
#6263 = APPROVAL_STATUS ( 'not_yet_approved' ) ;
#6264 = CIRCLE ( 'NONE', #11480, 0.7619999999999294005 ) ;
#6265 = CARTESIAN_POINT ( 'NONE',  ( 9.855201422231997910, -3639.502499925999928, 2279.447341858000073 ) ) ;
#6266 = DIRECTION ( 'NONE',  ( 0.000000000000000000, 0.000000000000000000, -1.000000000000000000 ) ) ;
#6267 = EDGE_CURVE ( 'NONE', #8402, #12177, #13715, .T. ) ;
#6268 = CARTESIAN_POINT ( 'NONE',  ( 12.69999999999999929, -3659.504999999999654, 2239.391000000000076 ) ) ;
#6269 = CARTESIAN_POINT ( 'NONE',  ( 111.4552000000009997, -3644.899999999999636, 2239.771999999999935 ) ) ;
#6270 = ORIENTED_EDGE ( 'NONE', *, *, #7385, .T. ) ;
#6271 = CARTESIAN_POINT ( 'NONE',  ( 136.7387998463173062, -3543.315277319925826, 2254.718298687770584 ) ) ;
#6272 = AXIS2_PLACEMENT_3D ( 'NONE', #7985, #2586, #16987 ) ;
#6273 = PERSON ( 'NAUO-PER8', 'UNSPECIFIED', 'UNSPECIFIED', ('UNSPECIFIED'), ('UNSPECIFIED'), ('UNSPECIFIED') ) ;
#6274 = EDGE_LOOP ( 'NONE', ( #16037, #17200, #20256, #19117 ) ) ;
#6275 = CARTESIAN_POINT ( 'NONE',  ( 140.6195432067733577, -3582.193521822282946, 2257.629402108334489 ) ) ;
#6276 = TOROIDAL_SURFACE ( 'NONE', #291, 3.606799999998999695, 0.7620000000000000107 ) ;
#6277 = DIRECTION ( 'NONE',  ( 0.000000000000000000, -1.000000000000000000, 0.000000000000000000 ) ) ;
#6278 = CIRCLE ( 'NONE', #19001, 1.904999999999823501 ) ;
#6279 = VERTEX_POINT ( 'NONE', #1115 ) ;
#6280 = ORIENTED_EDGE ( 'NONE', *, *, #4937, .T. ) ;
#6281 = DIRECTION ( 'NONE',  ( 0.000000000000000000, 0.000000000000000000, 1.000000000000000000 ) ) ;
#6282 = FACE_OUTER_BOUND ( 'NONE', #20277, .T. ) ;
#6283 = DIRECTION ( 'NONE',  ( 0.000000000000000000, -1.000000000000000000, 0.000000000000000000 ) ) ;
#6284 = ADVANCED_FACE ( 'NONE', ( #2646, #6529, #20813, #11907, #10029, #22786, #8515, #15661, #13317, #17878, #19762, #3459, #17518, #19518, #13902, #21397, #5346, #10377, #1823, #21050, #21288, #4995, #3692 ), #15775, .T. ) ;
#6285 = ADVANCED_FACE ( 'NONE', ( #8972 ), #20081, .T. ) ;
#6286 = CARTESIAN_POINT ( 'NONE',  ( -8.890000000008001280, -3661.486200000000281, 2249.723686796999573 ) ) ;
#6287 = LINE ( 'NONE', #1101, #6474 ) ;
#6288 = EDGE_CURVE ( 'NONE', #6818, #15892, #21199, .T. ) ;
#6289 = CARTESIAN_POINT ( 'NONE',  ( 20.79047622000200946, -3695.700000000006639, 2259.421674269511641 ) ) ;
#6290 = VERTEX_POINT ( 'NONE', #10612 ) ;
#6291 = PERSON_AND_ORGANIZATION_ROLE ( 'design_owner' ) ;
#6292 = CIRCLE ( 'NONE', #23110, 3.606800000000021100 ) ;
#6293 = DIRECTION ( 'NONE',  ( 0.000000000000000000, 1.000000000000000000, 0.000000000000000000 ) ) ;
#6294 = EDGE_CURVE ( 'NONE', #4732, #17234, #2849, .T. ) ;
#6295 = AXIS2_PLACEMENT_3D ( 'NONE', #23075, #7159, #21338 ) ;
#6296 = DIRECTION ( 'NONE',  ( -1.000000000000000000, 0.000000000000000000, 0.000000000000000000 ) ) ;
#6297 = CARTESIAN_POINT ( 'NONE',  ( 3.048000000000000043, -3695.699999999999818, 2238.248000000000047 ) ) ;
#6298 = EDGE_LOOP ( 'NONE', ( #13535, #9008, #8179, #4518, #9384, #3247, #10588, #13591 ) ) ;
#6299 = ADVANCED_FACE ( 'NONE', ( #3231 ), #1740, .T. ) ;
#6300 = CARTESIAN_POINT ( 'NONE',  ( 63.50000000000000000, -3644.899999999999636, 2239.771999999999935 ) ) ;
#6301 = EDGE_CURVE ( 'NONE', #19144, #1715, #14139, .T. ) ;
#6302 = FACE_OUTER_BOUND ( 'NONE', #17463, .T. ) ;
#6303 = DIRECTION ( 'NONE',  ( 0.000000000000000000, 0.000000000000000000, -1.000000000000000000 ) ) ;
#6304 = VERTEX_POINT ( 'NONE', #23134 ) ;
#6305 = LINE ( 'NONE', #14970, #9956 ) ;
#6306 = CARTESIAN_POINT ( 'NONE',  ( 14.63600372084860624, -3661.589906291256284, 2249.839665659381353 ) ) ;
#6307 = CIRCLE ( 'NONE', #17140, 3.606799999998994366 ) ;
#6308 = DIRECTION ( 'NONE',  ( -1.000000000000000000, 0.000000000000000000, 0.000000000000000000 ) ) ;
#6309 = VERTEX_POINT ( 'NONE', #10842 ) ;
#6310 = CARTESIAN_POINT ( 'NONE',  ( 35.56000000000000227, -3543.299999999999727, 2247.392000000000280 ) ) ;
#6311 = DIRECTION ( 'NONE',  ( 0.000000000000000000, -1.000000000000000000, 0.000000000000000000 ) ) ;
#6312 = EDGE_CURVE ( 'NONE', #14341, #9781, #6618, .T. ) ;
#6313 = CARTESIAN_POINT ( 'NONE',  ( 12.69999999999999929, -3659.504999999999654, 2239.009999999999764 ) ) ;
#6314 = CARTESIAN_POINT ( 'NONE',  ( 85.29320000000001301, -3644.899999999999636, 2239.771999999999935 ) ) ;
#6315 = DIRECTION ( 'NONE',  ( 0.000000000000000000, 1.000000000000000000, 0.000000000000000000 ) ) ;
#6316 = ORIENTED_EDGE ( 'NONE', *, *, #5146, .F. ) ;
#6317 = EDGE_LOOP ( 'NONE', ( #5504, #720 ) ) ;
#6318 = CARTESIAN_POINT ( 'NONE',  ( -12.70000000000007923, -3661.706170452909191, 2244.679313203225774 ) ) ;
#6319 = ORIENTED_EDGE ( 'NONE', *, *, #11634, .T. ) ;
#6320 = DIRECTION ( 'NONE',  ( 0.000000000000000000, 0.000000000000000000, -1.000000000000000000 ) ) ;
#6321 = CALENDAR_DATE ( 2026, 26, 10 ) ;
#6322 = CARTESIAN_POINT ( 'NONE',  ( 101.5999999999999943, -3568.700000000000273, 2259.837999999999738 ) ) ;
#6323 = CARTESIAN_POINT ( 'NONE',  ( 17.92468170931930160, -3661.821022282586000, 2245.096946498718353 ) ) ;
#6324 = AXIS2_PLACEMENT_3D ( 'NONE', #21617, #5570, #16218 ) ;
#6325 = CARTESIAN_POINT ( 'NONE',  ( 54.40679999999999694, -3619.500000000000000, 2259.837999999999738 ) ) ;
#6326 = CARTESIAN_POINT ( 'NONE',  ( 141.0563433985999779, -3581.844255679000071, 2239.391000000000076 ) ) ;
#6327 = DIRECTION ( 'NONE',  ( 0.000000000000000000, 1.000000000000000000, 0.000000000000000000 ) ) ;
#6328 = ORIENTED_EDGE ( 'NONE', *, *, #14021, .F. ) ;
#6329 = CARTESIAN_POINT ( 'NONE',  ( 114.2999999999999972, -3594.099999999999909, 2260.600000000000364 ) ) ;
#6330 = FACE_OUTER_BOUND ( 'NONE', #7796, .T. ) ;
#6331 = ORIENTED_EDGE ( 'NONE', *, *, #8379, .F. ) ;
#6332 = CARTESIAN_POINT ( 'NONE',  ( 127.0000000000000000, -3670.300000000000182, 2239.771999999999935 ) ) ;
#6333 = CARTESIAN_POINT ( 'NONE',  ( 10.84178118933141377, -3657.349603116384515, 2246.808232705630871 ) ) ;
#6334 = ORIENTED_EDGE ( 'NONE', *, *, #19767, .T. ) ;
#6335 = EDGE_LOOP ( 'NONE', ( #11595, #7951, #4611, #2206 ) ) ;
#6336 = ORIENTED_EDGE ( 'NONE', *, *, #1116, .F. ) ;
#6337 = COORDINATED_UNIVERSAL_TIME_OFFSET ( 0, 0, .AHEAD. ) ;
#6338 = DIRECTION ( 'NONE',  ( -2.343004830739999973E-14, -1.784212334590129905E-30, -1.000000000000000000 ) ) ;
#6339 = B_SPLINE_CURVE_WITH_KNOTS ( 'NONE', 3,
 ( #21423, #7025, #12164, #3257, #21542, #13924, #10403, #17543, #19785, #19544, #1851, #6784, #22925, #19430, #1489, #10632, #14393, #1607, #5021 ),
 .UNSPECIFIED., .F., .F.,
 ( 4, 1, 1, 1, 1, 1, 1, 1, 1, 1, 1, 1, 1, 1, 1, 1, 4 ),
 ( 0.000000000000000000, 0.06250000000000000000, 0.1250000000000000000, 0.1875000000000000000, 0.2500000000000000000, 0.3125000000000000000, 0.3750000000000000000, 0.4375000000000000000, 0.5000000000000000000, 0.5625000000000000000, 0.6250000000000000000, 0.6875000000000000000, 0.7500000000000000000, 0.8125000000000000000, 0.8750000000000000000, 0.9375000000000000000, 1.000000000000000000 ),
 .UNSPECIFIED. ) ;
#6340 = TOROIDAL_SURFACE ( 'NONE', #7457, 3.606799999999999784, 0.7620000000000000107 ) ;
#6341 = ORIENTED_EDGE ( 'NONE', *, *, #4065, .T. ) ;
#6342 = APPROVAL ( #18641, 'UNSPECIFIED' ) ;
#6343 = DIRECTION ( 'NONE',  ( 2.339144844575037611E-14, 0.000000000000000000, 1.000000000000000000 ) ) ;
#6344 = CARTESIAN_POINT ( 'NONE',  ( 13.90342121230041528, -3576.915831503414665, 2249.469455096983438 ) ) ;
#6345 = DIRECTION ( 'NONE',  ( 0.000000000000000000, 0.000000000000000000, 1.000000000000000000 ) ) ;
#6346 = CARTESIAN_POINT ( 'NONE',  ( 141.8951334675158478, -3581.304718316791423, 2248.847051393844140 ) ) ;
#6347 = EDGE_LOOP ( 'NONE', ( #14225, #17, #14345, #13794 ) ) ;
#6348 = DIRECTION ( 'NONE',  ( 0.000000000000000000, 0.000000000000000000, -1.000000000000000000 ) ) ;
#6349 = PERSON_AND_ORGANIZATION ( #5446, #1895 ) ;
#6350 = ADVANCED_FACE ( 'NONE', ( #19290, #10494 ), #17636, .F. ) ;
#6351 = CARTESIAN_POINT ( 'NONE',  ( 9.855200000000680305, -3579.043785370519799, 2256.063559999999597 ) ) ;
#6352 = LINE ( 'NONE', #13374, #22319 ) ;
#6353 = VECTOR ( 'NONE', #11544, 1000.000000000000000 ) ;
#6354 = EDGE_CURVE ( 'NONE', #20632, #15794, #14253, .T. ) ;
#6355 = CARTESIAN_POINT ( 'NONE',  ( 134.0034857541872100, -3659.043311792284385, 2244.766319695583661 ) ) ;
#6356 = ORIENTED_EDGE ( 'NONE', *, *, #13116, .F. ) ;
#6357 = TOROIDAL_SURFACE ( 'NONE', #14964, 5.080000000000000071, 0.3810000000000000053 ) ;
#6358 = CARTESIAN_POINT ( 'NONE',  ( -6.349999999999999645, -3544.061999999999898, 2253.487999999999829 ) ) ;
#6359 = ORIENTED_EDGE ( 'NONE', *, *, #5111, .T. ) ;
#6360 = ORIENTED_EDGE ( 'NONE', *, *, #10495, .F. ) ;
#6361 =( BOUNDED_CURVE ( )  B_SPLINE_CURVE ( 3, ( #18046, #7389, #14421, #9028 ),
 .UNSPECIFIED., .F., .T. ) 
 B_SPLINE_CURVE_WITH_KNOTS ( ( 4, 4 ),
 ( 1.570796326307487334, 3.141592653589783346 ),
 .UNSPECIFIED. ) 
 CURVE ( )  GEOMETRIC_REPRESENTATION_ITEM ( )  RATIONAL_B_SPLINE_CURVE ( ( 1.000000000000000000, 0.8047378540094838328, 0.8047378540094838328, 1.000000000000000000 ) ) 
 REPRESENTATION_ITEM ( '' )  );
#6362 = CARTESIAN_POINT ( 'NONE',  ( -12.31900000000012874, -3660.140000000000327, 2241.931000000000040 ) ) ;
#6363 = ORIENTED_EDGE ( 'NONE', *, *, #1847, .T. ) ;
#6364 = DIRECTION ( 'NONE',  ( 0.000000000000000000, 0.000000000000000000, 1.000000000000000000 ) ) ;
#6365 = DIRECTION ( 'NONE',  ( 0.000000000000000000, 1.000000000000000000, 5.827942386484301240E-13 ) ) ;
#6366 = VECTOR ( 'NONE', #2561, 1000.000000000000000 ) ;
#6367 = ORIENTED_EDGE ( 'NONE', *, *, #19271, .T. ) ;
#6368 = APPLIED_PERSON_AND_ORGANIZATION_ASSIGNMENT ( #9893, #11647, ( #3761 ) ) ;
#6369 = CARTESIAN_POINT ( 'NONE',  ( 12.69999999999999929, -3579.494999999999891, 2270.760000000000218 ) ) ;
#6370 = CYLINDRICAL_SURFACE ( 'NONE', #18078, 5.460999999999938126 ) ;
#6371 = APPROVAL_PERSON_ORGANIZATION ( #21595, #14222, #17598 ) ;
#6372 = LINE ( 'NONE', #2506, #17088 ) ;
#6373 = DATE_AND_TIME ( #6838, #18694 ) ;
#6374 = ADVANCED_FACE ( 'NONE', ( #8746 ), #23050, .T. ) ;
#6375 = FACE_OUTER_BOUND ( 'NONE', #16099, .T. ) ;
#6376 = CARTESIAN_POINT ( 'NONE',  ( 12.69999999994000106, -3636.370159094999508, 2296.591799999999694 ) ) ;
#6377 = DIRECTION ( 'NONE',  ( 0.000000000000000000, 0.000000000000000000, 1.000000000000000000 ) ) ;
#6378 = EDGE_CURVE ( 'NONE', #1694, #15010, #966, .T. ) ;
#6379 = EDGE_CURVE ( 'NONE', #1414, #1200, #20819, .T. ) ;
#6380 = CARTESIAN_POINT ( 'NONE',  ( 142.0115892277856631, -3657.846812289455102, 2249.075827970531918 ) ) ;
#6381 = LINE ( 'NONE', #9874, #4409 ) ;
#6382 = B_SPLINE_CURVE_WITH_KNOTS ( 'NONE', 3,
 ( #12912, #824, #18642, #2253 ),
 .UNSPECIFIED., .F., .F.,
 ( 4, 4 ),
 ( 0.9999948892526789868, 1.000000000000000000 ),
 .UNSPECIFIED. ) ;
#6383 = ORIENTED_EDGE ( 'NONE', *, *, #16561, .F. ) ;
#6384 = CARTESIAN_POINT ( 'NONE',  ( 136.9315409364155869, -3543.507962132184730, 2255.201583317368204 ) ) ;
#6385 = APPLIED_SECURITY_CLASSIFICATION_ASSIGNMENT ( #16481, ( #23168 ) ) ;
#6386 = ORIENTED_EDGE ( 'NONE', *, *, #7568, .T. ) ;
#6387 = CARTESIAN_POINT ( 'NONE',  ( -12.31900000000003459, -3581.552400000169200, 2247.392000000001190 ) ) ;
#6388 = DIRECTION ( 'NONE',  ( -1.000000000000000000, 1.206520773835000154E-12, 0.000000000000000000 ) ) ;
#6389 = ORIENTED_EDGE ( 'NONE', *, *, #13504, .F. ) ;
#6390 = ORIENTED_EDGE ( 'NONE', *, *, #8058, .T. ) ;
#6391 = ADVANCED_FACE ( 'NONE', ( #6995 ), #4156, .T. ) ;
#6392 = CARTESIAN_POINT ( 'NONE',  ( 18.41499991942999870, -3579.284285772028397, 2244.570689628976652 ) ) ;
#6393 = DIRECTION ( 'NONE',  ( 0.7249994335945011414, 0.000000000000000000, 0.6887494619146010688 ) ) ;
#6394 = LINE ( 'NONE', #20917, #5221 ) ;
#6395 = DIRECTION ( 'NONE',  ( -0.8660254037817188832, -0.5000000000047110094, 1.319534125263029996E-12 ) ) ;
#6396 = DIRECTION ( 'NONE',  ( 0.000000000000000000, 0.000000000000000000, 1.000000000000000000 ) ) ;
#6397 = ORIENTED_EDGE ( 'NONE', *, *, #19335, .T. ) ;
#6398 = PERSON_AND_ORGANIZATION ( #5446, #1895 ) ;
#6399 = ORIENTED_EDGE ( 'NONE', *, *, #19154, .T. ) ;
#6400 = CARTESIAN_POINT ( 'NONE',  ( 105.2067999999999870, -3568.700000000000273, 2239.009999999999764 ) ) ;
#6401 = LOCAL_TIME ( 17, 37, 43.00000000000000000, #4434 ) ;
#6402 = SECURITY_CLASSIFICATION ( '', '', #2046 ) ;
#6403 = ADVANCED_FACE ( 'NONE', ( #2180 ), #20106, .F. ) ;
#6404 = DIRECTION ( 'NONE',  ( 0.000000000000000000, -1.000000000000000000, 0.000000000000000000 ) ) ;
#6405 = CARTESIAN_POINT ( 'NONE',  ( 101.5999999999999943, -3670.300000000000182, 2239.009999999999764 ) ) ;
#6406 = ORIENTED_EDGE ( 'NONE', *, *, #9516, .T. ) ;
#6407 = CARTESIAN_POINT ( 'NONE',  ( 64.76999999999999602, -3694.938000000000102, 2292.057900000000245 ) ) ;
#6408 = ADVANCED_FACE ( 'NONE', ( #16351 ), #19871, .T. ) ;
#6409 = CIRCLE ( 'NONE', #15384, 3.606800000000000228 ) ;
#6410 = ADVANCED_FACE ( 'NONE', ( #3806 ), #1342, .T. ) ;
#6411 = DIRECTION ( 'NONE',  ( 0.000000000000000000, 0.000000000000000000, -1.000000000000000000 ) ) ;
#6412 = CARTESIAN_POINT ( 'NONE',  ( 144.5139337266538178, -3662.585492863386662, 2245.937534930569200 ) ) ;
#6413 = ORIENTED_EDGE ( 'NONE', *, *, #20193, .T. ) ;
#6414 = CARTESIAN_POINT ( 'NONE',  ( 15.54479972192533488, -3659.504999998566745, 2257.962943247991007 ) ) ;
#6415 = CARTESIAN_POINT ( 'NONE',  ( 13.89599138193900707, -3662.087915362755666, 2249.466105491610051 ) ) ;
#6416 = CARTESIAN_POINT ( 'NONE',  ( 25.39999999999999858, -3578.860000000000127, 2244.547199999999975 ) ) ;
#6417 = ORIENTED_EDGE ( 'NONE', *, *, #16738, .T. ) ;
#6418 = LOCAL_TIME ( 17, 37, 43.00000000000000000, #10711 ) ;
#6419 = ADVANCED_FACE ( 'NONE', ( #9326 ), #14714, .F. ) ;
#6420 = DIRECTION ( 'NONE',  ( 0.000000000000000000, -1.000000000000000000, 0.000000000000000000 ) ) ;
#6421 = CARTESIAN_POINT ( 'NONE',  ( 3.048000000000000043, -3543.299999999999727, 2238.248000000000047 ) ) ;
#6422 = CARTESIAN_POINT ( 'NONE',  ( 9.653865685812997199, -3581.600845684150045, 2246.629994766630261 ) ) ;
#6423 = CARTESIAN_POINT ( 'NONE',  ( 15.54461496037964174, -3659.404891253186179, 2250.142101673399793 ) ) ;
#6424 = CARTESIAN_POINT ( 'NONE',  ( 139.6999999999999886, -3664.965999999999894, 2244.978999999999814 ) ) ;
#6425 = ORIENTED_EDGE ( 'NONE', *, *, #4834, .F. ) ;
#6426 = AXIS2_PLACEMENT_3D ( 'NONE', #2083, #1962, #17897 ) ;
#6427 = EDGE_CURVE ( 'NONE', #18679, #22455, #6987, .T. ) ;
#6428 = ORIENTED_EDGE ( 'NONE', *, *, #12670, .F. ) ;
#6429 = CIRCLE ( 'NONE', #3424, 6.349999999999855760 ) ;
#6430 = FACE_OUTER_BOUND ( 'NONE', #8159, .T. ) ;
#6431 = VERTEX_POINT ( 'NONE', #4271 ) ;
#6432 = CARTESIAN_POINT ( 'NONE',  ( 15.53591867179932073, -3579.770168290938727, 2257.960586820520803 ) ) ;
#6433 = APPROVAL_DATE_TIME ( #13452, #4322 ) ;
#6434 = DIRECTION ( 'NONE',  ( 0.000000000000000000, 0.000000000000000000, -1.000000000000000000 ) ) ;
#6435 = DIRECTION ( 'NONE',  ( 0.000000000000000000, 0.000000000000000000, -1.000000000000000000 ) ) ;
#6436 = CARTESIAN_POINT ( 'NONE',  ( 12.69999999999999929, -3579.494999999999891, 2244.978999999999814 ) ) ;
#6437 = CARTESIAN_POINT ( 'NONE',  ( 12.69999999999999929, -3653.789999999999964, 2268.705139999999574 ) ) ;
#6438 = DIRECTION ( 'NONE',  ( -1.000000000000000000, 0.000000000000000000, 0.000000000000000000 ) ) ;
#6439 = ADVANCED_FACE ( 'NONE', ( #4044 ), #7449, .F. ) ;
#6440 = CARTESIAN_POINT ( 'NONE',  ( 15.41268679713999923, -3641.068670452857532, 2296.591799999999694 ) ) ;
#6441 = VERTEX_POINT ( 'NONE', #14599 ) ;
#6442 = CIRCLE ( 'NONE', #5696, 5.080000000000000959 ) ;
#6443 = CARTESIAN_POINT ( 'NONE',  ( 7.327249423652832050, -3657.550365826240522, 2246.178457032339793 ) ) ;
#6444 = TOROIDAL_SURFACE ( 'NONE', #1562, 7.112000000000000099, 0.7620000000000000107 ) ;
#6445 = FACE_OUTER_BOUND ( 'NONE', #758, .T. ) ;
#6446 = VERTEX_POINT ( 'NONE', #11409 ) ;
#6447 = CARTESIAN_POINT ( 'NONE',  ( 47.95519999999999783, -3670.300000000000182, 2261.869999999999891 ) ) ;
#6448 = CARTESIAN_POINT ( 'NONE',  ( 10.37279685983138400, -3657.868421124709130, 2249.105504558603570 ) ) ;
#6449 = ORIENTED_EDGE ( 'NONE', *, *, #7240, .T. ) ;
#6450 = ORIENTED_EDGE ( 'NONE', *, *, #20754, .F. ) ;
#6451 = CARTESIAN_POINT ( 'NONE',  ( 134.0869790975583840, -3580.606330659021751, 2245.129232553249949 ) ) ;
#6452 = PRODUCT_DEFINITION_CONTEXT ( 'detailed design', #8873, 'design' ) ;
#6453 = VECTOR ( 'NONE', #7129, 1000.000000000000000 ) ;
#6454 = EDGE_CURVE ( 'NONE', #13782, #13805, #9660, .T. ) ;
#6455 = ORIENTED_EDGE ( 'NONE', *, *, #19921, .T. ) ;
#6456 = DIRECTION ( 'NONE',  ( 1.000000000000000000, 0.000000000000000000, 8.741913579725999495E-14 ) ) ;
#6457 = CARTESIAN_POINT ( 'NONE',  ( 10.57279766787198838, -3577.605992114683886, 2249.945558813966727 ) ) ;
#6458 = CARTESIAN_POINT ( 'NONE',  ( 0.000000000000000000, 0.000000000000000000, 0.000000000000000000 ) ) ;
#6459 = CARTESIAN_POINT ( 'NONE',  ( 141.8303725231117198, -3581.380460283721277, 2248.711714140399636 ) ) ;
#6460 = AXIS2_PLACEMENT_3D ( 'NONE', #13832, #10189, #22603 ) ;
#6461 = VERTEX_POINT ( 'NONE', #14829 ) ;
#6463 = CARTESIAN_POINT ( 'NONE',  ( 137.9608668947936110, -3581.754029086221635, 2257.728452929456580 ) ) ;
#6462 = AXIS2_PLACEMENT_3D ( 'NONE', #3950, #14391, #14278 ) ;
#6464 = PERSON_AND_ORGANIZATION ( #5446, #1895 ) ;
#6465 = DIRECTION ( 'NONE',  ( -0.8660254037815640071, 0.5000000000049790172, 0.000000000000000000 ) ) ;
#6466 = DIRECTION ( 'NONE',  ( 0.000000000000000000, 0.000000000000000000, 1.000000000000000000 ) ) ;
#6467 = CARTESIAN_POINT ( 'NONE',  ( 133.9850000806000025, -3659.390917837453344, 2244.645117375718655 ) ) ;
#6468 = ORIENTED_EDGE ( 'NONE', *, *, #7737, .T. ) ;
#6469 = CIRCLE ( 'NONE', #1590, 2.844799999999994444 ) ;
#6470 = CYLINDRICAL_SURFACE ( 'NONE', #2097, 3.175000000000149925 ) ;
#6471 = APPLIED_DATE_AND_TIME_ASSIGNMENT ( #1735, #22922, ( #16852 ) ) ;
#6472 = VERTEX_POINT ( 'NONE', #21857 ) ;
#6473 = LINE ( 'NONE', #3058, #10991 ) ;
#6474 = VECTOR ( 'NONE', #13302, 1000.000000000000000 ) ;
#6475 = CIRCLE ( 'NONE', #8345, 11.11250000000000071 ) ;
#6476 = APPLICATION_CONTEXT ( 'configuration controlled 3d designs of mechanical parts and assemblies' ) ;
#6477 = DIRECTION ( 'NONE',  ( 0.000000000000000000, -1.000000000000000000, 0.000000000000000000 ) ) ;
#6478 = ORIENTED_EDGE ( 'NONE', *, *, #8857, .T. ) ;
#6479 = LINE ( 'NONE', #20763, #4929 ) ;
#6480 = DIRECTION ( 'NONE',  ( 0.000000000000000000, 1.000000000000000000, 0.000000000000000000 ) ) ;
#6481 = ORIENTED_EDGE ( 'NONE', *, *, #17985, .T. ) ;
#6482 = AXIS2_PLACEMENT_3D ( 'NONE', #15184, #18685, #2634 ) ;
#6483 = CARTESIAN_POINT ( 'NONE',  ( 139.7000000001000046, -3576.802599999999984, 2242.820000000000164 ) ) ;
#6484 =( NAMED_UNIT ( * ) PLANE_ANGLE_UNIT ( ) SI_UNIT ( $, .RADIAN. ) );
#6485 = CARTESIAN_POINT ( 'NONE',  ( 13.92840658401000020, -3602.070073557999876, 2279.750815596999928 ) ) ;
#6486 = CARTESIAN_POINT ( 'NONE',  ( -5.588000000000000078, -3544.061999999999898, 2228.849999999999909 ) ) ;
#6487 = TOROIDAL_SURFACE ( 'NONE', #130, 3.606799999998999695, 0.7620000000000000107 ) ;
#6488 = PERSON_AND_ORGANIZATION ( #5446, #1895 ) ;
#6489 = DIRECTION ( 'NONE',  ( 0.000000000000000000, 1.000000000000000000, 0.000000000000000000 ) ) ;
#6490 = DIRECTION ( 'NONE',  ( 1.224646799147353207E-16, 1.000000000000000000, -0.000000000000000000 ) ) ;
#6491 = CARTESIAN_POINT ( 'NONE',  ( 28.24479999999899604, -3568.700000000000273, 2259.837999999999738 ) ) ;
#6492 = CIRCLE ( 'NONE', #3858, 0.7619999999999294005 ) ;
#6493 = CLOSED_SHELL ( 'NONE', ( #3428, #6010, #14702, #18725, #10489, #5668, #8281, #15263, #18664, #6087, #8655, #18308, #2373, #17877, #18317, #10060, #10520, #12829, #13709, #2959, #19324, #18503, #5270, #12378, #6299, #20042 ) ) ;
#6494 = CARTESIAN_POINT ( 'NONE',  ( 141.7685968712770261, -3657.550763801919857, 2248.576229848027651 ) ) ;
#6495 = CARTESIAN_POINT ( 'NONE',  ( -5.588000000000000078, -3695.699999999999818, 2229.612000000000080 ) ) ;
#6496 = EDGE_LOOP ( 'NONE', ( #15660, #13233, #7820, #18933 ) ) ;
#6497 = DIRECTION ( 'NONE',  ( 0.000000000000000000, 0.000000000000000000, -1.000000000000000000 ) ) ;
#6498 = APPLIED_DATE_AND_TIME_ASSIGNMENT ( #17979, #3795, ( #13135 ) ) ;
#6499 = ORIENTED_EDGE ( 'NONE', *, *, #2969, .F. ) ;
#6500 = AXIS2_PLACEMENT_3D ( 'NONE', #20919, #10668, #12077 ) ;
#6501 = CARTESIAN_POINT ( 'NONE',  ( 9.855200958505918152, -3579.586994900638729, 2257.962940081783472 ) ) ;
#6502 = CYLINDRICAL_SURFACE ( 'NONE', #4718, 0.7619999999999294005 ) ;
#6503 = ADVANCED_FACE ( 'NONE', ( #21962 ), #13065, .F. ) ;
#6504 = ORIENTED_EDGE ( 'NONE', *, *, #14174, .T. ) ;
#6505 = ORIENTED_EDGE ( 'NONE', *, *, #17551, .F. ) ;
#6506 = CARTESIAN_POINT ( 'NONE',  ( 76.20000000000000284, -3670.300000000000182, 2239.009999999999764 ) ) ;
#6507 = EDGE_CURVE ( 'NONE', #20457, #4775, #7365, .T. ) ;
#6508 = DIRECTION ( 'NONE',  ( -2.336881798971000105E-14, 0.000000000000000000, -1.000000000000000000 ) ) ;
#6509 = CARTESIAN_POINT ( 'NONE',  ( 12.69999999999999929, -3599.497499999999945, 2263.571799999999712 ) ) ;
#6510 = EDGE_CURVE ( 'NONE', #9415, #17185, #13731, .T. ) ;
#6511 = VERTEX_POINT ( 'NONE', #21742 ) ;
#6512 = AXIS2_PLACEMENT_3D ( 'NONE', #7856, #6107, #4446 ) ;
#6513 = CARTESIAN_POINT ( 'NONE',  ( 15.03168679706412902, -3638.156299999897783, 2296.210799999999836 ) ) ;
#6514 = CARTESIAN_POINT ( 'NONE',  ( 114.2999999999999972, -3644.899999999999636, 2239.009999999999764 ) ) ;
#6515 = CARTESIAN_POINT ( 'NONE',  ( 139.5113177728721610, -3656.660200000000714, 2257.592639999999847 ) ) ;
#6516 = CARTESIAN_POINT ( 'NONE',  ( 0.7620000000000000107, -3694.938000000000102, 2238.248000000000047 ) ) ;
#6517 = ORIENTED_EDGE ( 'NONE', *, *, #9962, .T. ) ;
#6518 = PERSON_AND_ORGANIZATION ( #5446, #1895 ) ;
#6519 = EDGE_LOOP ( 'NONE', ( #10032, #9595, #3668 ) ) ;
#6520 = EDGE_CURVE ( 'NONE', #19601, #9977, #2867, .T. ) ;
#6521 = DIRECTION ( 'NONE',  ( 0.000000000000000000, 0.000000000000000000, -1.000000000000000000 ) ) ;
#6522 = AXIS2_PLACEMENT_3D ( 'NONE', #22355, #16751, #4667 ) ;
#6523 = AXIS2_PLACEMENT_3D ( 'NONE', #6748, #12009, #4980 ) ;
#6524 = CARTESIAN_POINT ( 'NONE',  ( 10.59346086370990037, -3581.406909921530314, 2248.659345565240528 ) ) ;
#6525 = ORIENTED_EDGE ( 'NONE', *, *, #16030, .F. ) ;
#6526 = DIRECTION ( 'NONE',  ( 1.000000000000000000, 0.000000000000000000, 0.000000000000000000 ) ) ;
#6527 = ADVANCED_FACE ( 'NONE', ( #22070 ), #5697, .T. ) ;
#6528 = EDGE_LOOP ( 'NONE', ( #11109, #10813, #20302, #11801 ) ) ;
#6529 = FACE_BOUND ( 'NONE', #18193, .T. ) ;
#6530 = ADVANCED_FACE ( 'NONE', ( #11074 ), #22701, .T. ) ;
#6531 = CARTESIAN_POINT ( 'NONE',  ( 38.10000000000000142, -3594.099999999999909, 2259.837999999999738 ) ) ;
#6532 = CARTESIAN_POINT ( 'NONE',  ( 145.3468180090523845, -3660.390156501248839, 2244.556611876515490 ) ) ;
#6533 = LINE ( 'NONE', #13433, #5537 ) ;
#6534 = CARTESIAN_POINT ( 'NONE',  ( 139.6999999999999886, -3579.494999999999891, 2239.391000000000076 ) ) ;
#6535 = FACE_OUTER_BOUND ( 'NONE', #14548, .T. ) ;
#6536 = ORIENTED_EDGE ( 'NONE', *, *, #4432, .T. ) ;
#6537 = DIRECTION ( 'NONE',  ( 1.000000000000000000, 0.000000000000000000, 0.000000000000000000 ) ) ;
#6538 = AXIS2_PLACEMENT_3D ( 'NONE', #8045, #13547, #15197 ) ;
#6539 = CARTESIAN_POINT ( 'NONE',  ( 15.39424581079000021, -3638.570999367999775, 2279.486256121999759 ) ) ;
#6540 = EDGE_CURVE ( 'NONE', #7171, #1044, #12225, .T. ) ;
#6541 = CARTESIAN_POINT ( 'NONE',  ( 57.14999999999999858, -3568.700000000000273, 2250.236800000000130 ) ) ;
#6542 = VECTOR ( 'NONE', #10387, 1000.000000000000000 ) ;
#6543 = CARTESIAN_POINT ( 'NONE',  ( 15.53944468019864722, -3659.305298452004081, 2250.113581315974443 ) ) ;
#6544 = CARTESIAN_POINT ( 'NONE',  ( 7.619999999999999218, -3639.502500000000055, 2296.591799999999694 ) ) ;
#6545 = ORIENTED_EDGE ( 'NONE', *, *, #20342, .T. ) ;
#6546 = ORIENTED_EDGE ( 'NONE', *, *, #17095, .T. ) ;
#6547 = CARTESIAN_POINT ( 'NONE',  ( 50.79999999999999716, -3670.300000000000182, 2239.771999999999935 ) ) ;
#6548 = ORIENTED_EDGE ( 'NONE', *, *, #21107, .F. ) ;
#6549 = CARTESIAN_POINT ( 'NONE',  ( 13.24911585008999815, -3582.290876935000142, 2257.605101898000157 ) ) ;
#6550 = COORDINATED_UNIVERSAL_TIME_OFFSET ( 0, 0, .AHEAD. ) ;
#6551 = DIRECTION ( 'NONE',  ( 0.000000000000000000, -1.000000000000000000, 0.000000000000000000 ) ) ;
#6552 = DIRECTION ( 'NONE',  ( 0.000000000000000000, -1.000000000000000000, 0.000000000000000000 ) ) ;
#6553 = PLANE ( 'NONE',  #19686 ) ;
#6554 = AXIS2_PLACEMENT_3D ( 'NONE', #12585, #19614, #12696 ) ;
#6555 = B_SPLINE_CURVE_WITH_KNOTS ( 'NONE', 3,
 ( #15875, #15521, #6982, #19393 ),
 .UNSPECIFIED., .F., .F.,
 ( 4, 4 ),
 ( 0.000000000000000000, 1.000000000000000000 ),
 .UNSPECIFIED. ) ;
#6556 = AXIS2_PLACEMENT_3D ( 'NONE', #18449, #15057, #743 ) ;
#6557 = CARTESIAN_POINT ( 'NONE',  ( 15.54479972196000048, -3659.504985917999875, 2257.962943248000101 ) ) ;
#6558 = VECTOR ( 'NONE', #1392, 1000.000000000000000 ) ;
#6559 = DIRECTION ( 'NONE',  ( 9.756599977372053330E-14, 0.000000000000000000, -1.000000000000000000 ) ) ;
#6560 = CIRCLE ( 'NONE', #11407, 0.7619999999999294005 ) ;
#6561 = CARTESIAN_POINT ( 'NONE',  ( 137.6199520187697090, -3577.554138631957812, 2249.919443248165862 ) ) ;
#6562 = ORIENTED_EDGE ( 'NONE', *, *, #22824, .T. ) ;
#6563 = CARTESIAN_POINT ( 'NONE',  ( 7.238999999999998991, -3579.494999999999891, 2244.978999999999814 ) ) ;
#6564 = DIRECTION ( 'NONE',  ( 0.000000000000000000, 0.000000000000000000, -1.000000000000000000 ) ) ;
#6565 = ORIENTED_EDGE ( 'NONE', *, *, #21463, .F. ) ;
#6566 = DIRECTION ( 'NONE',  ( -1.000000000000000000, 2.330758767201999921E-14, 2.343004830739999973E-14 ) ) ;
#6567 = FACE_OUTER_BOUND ( 'NONE', #19224, .T. ) ;
#6568 = ORIENTED_EDGE ( 'NONE', *, *, #8238, .F. ) ;
#6569 = ORIENTED_EDGE ( 'NONE', *, *, #18147, .T. ) ;
#6570 = FACE_OUTER_BOUND ( 'NONE', #11753, .T. ) ;
#6571 = TOROIDAL_SURFACE ( 'NONE', #20406, 3.606799999999999784, 0.7620000000000000107 ) ;
#6572 = AXIS2_PLACEMENT_3D ( 'NONE', #13822, #8660, #1390 ) ;
#6573 = ORIENTED_EDGE ( 'NONE', *, *, #19115, .F. ) ;
#6574 = AXIS2_PLACEMENT_3D ( 'NONE', #6310, #8286, #22446 ) ;
#6575 = CARTESIAN_POINT ( 'NONE',  ( 35.25520000000000209, -3644.899999999999636, 2239.771999999999935 ) ) ;
#6576 = EDGE_CURVE ( 'NONE', #8944, #19446, #11750, .T. ) ;
#6577 = CARTESIAN_POINT ( 'NONE',  ( 72.59320000000001016, -3670.300000000000182, 2239.009999999999764 ) ) ;
#6578 = AXIS2_PLACEMENT_3D ( 'NONE', #19825, #3753, #368 ) ;
#6579 = EDGE_CURVE ( 'NONE', #13032, #23163, #6151, .T. ) ;
#6580 = DIRECTION ( 'NONE',  ( 1.000000000000000000, 0.000000000000000000, 0.000000000000000000 ) ) ;
#6581 = ORIENTED_EDGE ( 'NONE', *, *, #15729, .T. ) ;
#6582 = CARTESIAN_POINT ( 'NONE',  ( 131.7716230377726561, -3695.598599741984799, 2259.827559975022723 ) ) ;
#6583 = PERSON_AND_ORGANIZATION_ROLE ( 'creator' ) ;
#6584 = DIRECTION ( 'NONE',  ( 2.330758767201999921E-14, 1.000000000000000000, -5.460979050843892707E-28 ) ) ;
#6585 = CARTESIAN_POINT ( 'NONE',  ( 14.50824192230427201, -3581.691173654184695, 2247.673267903098349 ) ) ;
#6586 = EDGE_CURVE ( 'NONE', #13767, #7997, #8368, .T. ) ;
#6587 = CARTESIAN_POINT ( 'NONE',  ( 134.0238007392231623, -3658.840387854182609, 2244.861395050478677 ) ) ;
#6588 = AXIS2_PLACEMENT_3D ( 'NONE', #13796, #21184, #10505 ) ;
#6589 = ORIENTED_EDGE ( 'NONE', *, *, #16954, .T. ) ;
#6590 = AXIS2_PLACEMENT_3D ( 'NONE', #191, #18226, #1832 ) ;
#6591 = DIRECTION ( 'NONE',  ( 0.000000000000000000, 1.000000000000000000, 0.000000000000000000 ) ) ;
#6592 = EDGE_CURVE ( 'NONE', #7259, #14462, #2730, .T. ) ;
#6593 = AXIS2_PLACEMENT_3D ( 'NONE', #2670, #22351, #3139 ) ;
#6594 = EDGE_CURVE ( 'NONE', #8860, #10297, #20780, .T. ) ;
#6596 = AXIS2_PLACEMENT_3D ( 'NONE', #21206, #5152, #6684 ) ;
#6595 = CARTESIAN_POINT ( 'NONE',  ( 12.69998522105610483, -3596.652698770827556, 2279.817639764999967 ) ) ;
#6597 = ORIENTED_EDGE ( 'NONE', *, *, #17435, .F. ) ;
#6598 = LINE ( 'NONE', #13737, #6132 ) ;
#6599 = AXIS2_PLACEMENT_3D ( 'NONE', #1293, #8461, #10436 ) ;
#6600 = CARTESIAN_POINT ( 'NONE',  ( 114.2999999999999972, -3644.899999999999636, 2259.837999999999738 ) ) ;
#6601 = VECTOR ( 'NONE', #8323, 1000.000000000000000 ) ;
#6602 = EDGE_LOOP ( 'NONE', ( #4992, #22313, #10953, #651 ) ) ;
#6603 = ORIENTED_EDGE ( 'NONE', *, *, #16122, .T. ) ;
#6604 = CARTESIAN_POINT ( 'NONE',  ( 139.6999999999986528, -3582.187400000082107, 2239.391000000000076 ) ) ;
#6605 = CARTESIAN_POINT ( 'NONE',  ( 133.9850000806000025, -3659.504501929000071, 2244.618659328000376 ) ) ;
#6606 = ORIENTED_EDGE ( 'NONE', *, *, #15595, .F. ) ;
#6607 = LINE ( 'NONE', #1657, #10972 ) ;
#6608 = CARTESIAN_POINT ( 'NONE',  ( 12.69999999999999929, -3648.710000000000036, 2268.705139999999574 ) ) ;
#6609 = CARTESIAN_POINT ( 'NONE',  ( 14.21033034659000016, -3601.915435226000227, 2279.715679318999719 ) ) ;
#6610 = CIRCLE ( 'NONE', #14075, 0.7619999999999987894 ) ;
#6611 = AXIS2_PLACEMENT_3D ( 'NONE', #17498, #3317, #17731 ) ;
#6612 = CARTESIAN_POINT ( 'NONE',  ( 1.270000000000000018, -3660.140000000000327, 2247.392000000000280 ) ) ;
#6613 = PERSON_AND_ORGANIZATION ( #5446, #1895 ) ;
#6614 = AXIS2_PLACEMENT_3D ( 'NONE', #6369, #627, #6141 ) ;
#6615 = DIRECTION ( 'NONE',  ( 0.000000000000000000, 0.000000000000000000, 1.000000000000000000 ) ) ;
#6616 = CARTESIAN_POINT ( 'NONE',  ( 56.10057940169000545, -3694.938000000000102, 2275.211350432000472 ) ) ;
#6617 = CARTESIAN_POINT ( 'NONE',  ( -8.890000000017000303, -3658.793800000000374, 2249.723686796999573 ) ) ;
#6618 = CIRCLE ( 'NONE', #21565, 3.606799999999001027 ) ;
#6619 = CARTESIAN_POINT ( 'NONE',  ( 141.6144402965059896, -3657.400733319522260, 2248.159976633087354 ) ) ;
#6620 = VECTOR ( 'NONE', #22330, 1000.000000000000000 ) ;
#6621 = ORIENTED_EDGE ( 'NONE', *, *, #12807, .T. ) ;
#6622 = CARTESIAN_POINT ( 'NONE',  ( 137.0608862933557077, -3543.814512435404595, 2255.525687528578146 ) ) ;
#6623 = ORIENTED_EDGE ( 'NONE', *, *, #15321, .T. ) ;
#6624 = CARTESIAN_POINT ( 'NONE',  ( 4.707381495575098995, -3695.655085019853232, 2259.667485322372613 ) ) ;
#6625 = CIRCLE ( 'NONE', #19722, 1.904999999999823501 ) ;
#6626 = DIRECTION ( 'NONE',  ( -3.424927947642999691E-13, 2.590196616237999979E-13, -1.000000000000000000 ) ) ;
#6627 = VERTEX_POINT ( 'NONE', #1202 ) ;
#6628 = EDGE_LOOP ( 'NONE', ( #6910, #18605, #6109, #6855 ) ) ;
#6629 = FACE_OUTER_BOUND ( 'NONE', #16451, .T. ) ;
#6630 = DIRECTION ( 'NONE',  ( 5.432398939370942693E-28, 1.000000000000000000, 2.336881798971000105E-14 ) ) ;
#6631 = CIRCLE ( 'NONE', #9611, 2.844800000000001550 ) ;
#6632 = CYLINDRICAL_SURFACE ( 'NONE', #10710, 3.175000000000149925 ) ;
#6633 = ORIENTED_EDGE ( 'NONE', *, *, #4147, .T. ) ;
#6634 = CARTESIAN_POINT ( 'NONE',  ( 21.79320000000099711, -3568.700000000000273, 2260.600000000000364 ) ) ;
#6635 = CARTESIAN_POINT ( 'NONE',  ( 3.048000000000000043, -3544.061999999999898, 2238.248000000000047 ) ) ;
#6636 = PLANE ( 'NONE',  #11344 ) ;
#6637 = CARTESIAN_POINT ( 'NONE',  ( 17.68024974314568354, -3576.692299003124390, 2245.542863885450970 ) ) ;
#6638 = CYLINDRICAL_SURFACE ( 'NONE', #6523, 0.3809999999999647002 ) ;
#6639 = EDGE_LOOP ( 'NONE', ( #23127, #4215, #602, #10794 ) ) ;
#6640 = PERSON_AND_ORGANIZATION_ROLE ( 'classification_officer' ) ;
#6641 = APPLIED_PERSON_AND_ORGANIZATION_ASSIGNMENT ( #14911, #9734, ( #3363 ) ) ;
#6642 = VERTEX_POINT ( 'NONE', #22183 ) ;
#6643 = DIRECTION ( 'NONE',  ( -1.000000000000000000, 0.000000000000000000, 0.000000000000000000 ) ) ;
#6644 =( BOUNDED_CURVE ( )  B_SPLINE_CURVE ( 3, ( #1665, #23101, #1900, #19723 ),
 .UNSPECIFIED., .F., .F. ) 
 B_SPLINE_CURVE_WITH_KNOTS ( ( 4, 4 ),
 ( -9.769962616701377556E-15, 1.570796326938358911 ),
 .UNSPECIFIED. ) 
 CURVE ( )  GEOMETRIC_REPRESENTATION_ITEM ( )  RATIONAL_B_SPLINE_CURVE ( ( 1.000000000000000000, 0.8047378540905483213, 0.8047378540905483213, 1.000000000000000000 ) ) 
 REPRESENTATION_ITEM ( '' )  );
#6645 = CARTESIAN_POINT ( 'NONE',  ( 10.34642913787651075, -3581.093266999223033, 2249.155114352099645 ) ) ;
#6646 = ADVANCED_FACE ( 'NONE', ( #974 ), #15607, .T. ) ;
#6647 = DIRECTION ( 'NONE',  ( 1.278298683860999806E-12, -1.000000000000000000, 0.000000000000000000 ) ) ;
#6648 = EDGE_CURVE ( 'NONE', #13538, #6235, #17448, .T. ) ;
#6649 = ORIENTED_EDGE ( 'NONE', *, *, #3183, .T. ) ;
#6650 = CARTESIAN_POINT ( 'NONE',  ( 97.99320000000000164, -3568.700000000000273, 2259.837999999999738 ) ) ;
#6651 = EDGE_CURVE ( 'NONE', #15032, #10096, #18275, .T. ) ;
#6652 = VECTOR ( 'NONE', #20181, 1000.000000000000000 ) ;
#6653 = CARTESIAN_POINT ( 'NONE',  ( 139.7000000001000046, -3576.802599999999984, 2242.820000000000164 ) ) ;
#6654 = CARTESIAN_POINT ( 'NONE',  ( 145.3761492408112872, -3660.170703703051913, 2244.547341334182875 ) ) ;
#6655 = CARTESIAN_POINT ( 'NONE',  ( 12.70000000005999929, -3576.802599999999984, 2242.820000000000164 ) ) ;
#6656 = CARTESIAN_POINT ( 'NONE',  ( 11.08609301964814264, -3661.848501376024615, 2249.666901776545728 ) ) ;
#6657 = CARTESIAN_POINT ( 'NONE',  ( 147.3229993024389728, -3544.409801988681920, 2260.592426251218058 ) ) ;
#6658 = VERTEX_POINT ( 'NONE', #16797 ) ;
#6659 = DIRECTION ( 'NONE',  ( 0.000000000000000000, -1.000000000000000000, 0.000000000000000000 ) ) ;
#6660 = PLANE ( 'NONE',  #8825 ) ;
#6661 = AXIS2_PLACEMENT_3D ( 'NONE', #10657, #3736, #5275 ) ;
#6662 = CARTESIAN_POINT ( 'NONE',  ( 136.8791170170333089, -3659.931058367113565, 2250.236800312005471 ) ) ;
#6663 = CARTESIAN_POINT ( 'NONE',  ( 14.51094036875449866, -3657.306545957249909, 2246.963123837074363 ) ) ;
#6664 = CARTESIAN_POINT ( 'NONE',  ( 12.69999999999999929, -3639.502500000000055, 2263.571799999999712 ) ) ;
#6665 = VERTEX_POINT ( 'NONE', #11627 ) ;
#6666 = ORIENTED_EDGE ( 'NONE', *, *, #2556, .T. ) ;
#6667 = AXIS2_PLACEMENT_3D ( 'NONE', #21736, #12832, #11070 ) ;
#6668 = CIRCLE ( 'NONE', #21704, 1.240967364599221412 ) ;
#6669 = DIRECTION ( 'NONE',  ( 0.000000000000000000, 0.000000000000000000, -1.000000000000000000 ) ) ;
#6670 = ORIENTED_EDGE ( 'NONE', *, *, #5876, .F. ) ;
#6671 = CARTESIAN_POINT ( 'NONE',  ( 142.4535506707765649, -3658.766509067717379, 2257.939127563549391 ) ) ;
#6672 = COORDINATED_UNIVERSAL_TIME_OFFSET ( 0, 0, .AHEAD. ) ;
#6673 = DIRECTION ( 'NONE',  ( 0.000000000000000000, 0.000000000000000000, 1.000000000000000000 ) ) ;
#6674 = EDGE_CURVE ( 'NONE', #22687, #11227, #3997, .T. ) ;
#6675 = CARTESIAN_POINT ( 'NONE',  ( 25.39999999999999858, -3670.300000000000182, 2239.771999999999935 ) ) ;
#6676 = CARTESIAN_POINT ( 'NONE',  ( 9.864080040025308804, -3659.780148078739330, 2257.960588549625299 ) ) ;
#6677 = EDGE_CURVE ( 'NONE', #11227, #12638, #8485, .T. ) ;
#6678 = CARTESIAN_POINT ( 'NONE',  ( 15.42952381853999988, -3658.687498958000106, 2257.932973515999947 ) ) ;
#6679 = ADVANCED_FACE ( 'NONE', ( #6848 ), #10343, .T. ) ;
#6680 = CARTESIAN_POINT ( 'NONE',  ( 60.65520000000000067, -3594.099999999999909, 2259.837999999999738 ) ) ;
#6681 = AXIS2_PLACEMENT_3D ( 'NONE', #17253, #1194, #21875 ) ;
#6682 = CARTESIAN_POINT ( 'NONE',  ( 57.14999999999999858, -3670.300000000000182, 2247.392000000000280 ) ) ;
#6683 = ORIENTED_EDGE ( 'NONE', *, *, #3990, .T. ) ;
#6684 = DIRECTION ( 'NONE',  ( -1.000000000000000000, 0.000000000000000000, 0.000000000000000000 ) ) ;
#6685 = CARTESIAN_POINT ( 'NONE',  ( 139.6999999999986528, -3662.197400000082780, 2239.391000000000076 ) ) ;
#6686 = EDGE_LOOP ( 'NONE', ( #19813, #16796, #16391, #8720, #15678, #5613, #15869, #15023, #14698 ) ) ;
#6687 = DIRECTION ( 'NONE',  ( 0.000000000000000000, 0.000000000000000000, -1.000000000000000000 ) ) ;
#6688 = CARTESIAN_POINT ( 'NONE',  ( 10.29010022044823458, -3657.993389994380777, 2249.258804498657810 ) ) ;
#6689 = ORIENTED_EDGE ( 'NONE', *, *, #3261, .F. ) ;
#6690 = ORIENTED_EDGE ( 'NONE', *, *, #15662, .F. ) ;
#6691 = CARTESIAN_POINT ( 'NONE',  ( 134.2892388165611521, -3581.334923857996728, 2245.989158447333466 ) ) ;
#6692 = PRODUCT_DEFINITION_CONTEXT ( 'detailed design', #1255, 'design' ) ;
#6693 = EDGE_LOOP ( 'NONE', ( #19902, #4959, #19260, #20104 ) ) ;
#6694 = LINE ( 'NONE', #22831, #3978 ) ;
#6695 = DIRECTION ( 'NONE',  ( 0.000000000000000000, 0.000000000000000000, 1.000000000000000000 ) ) ;
#6696 = CARTESIAN_POINT ( 'NONE',  ( -0.7619999999998999796, -3695.699999999999818, 2239.771999999999935 ) ) ;
#6697 = ORIENTED_EDGE ( 'NONE', *, *, #22559, .T. ) ;
#6698 = CARTESIAN_POINT ( 'NONE',  ( 131.9612844717763664, -3695.249961889823680, 2260.302094140601184 ) ) ;
#6699 = APPLICATION_PROTOCOL_DEFINITION ( 'international standard', 'automotive_design', 2000, #22469 ) ;
#6700 = CARTESIAN_POINT ( 'NONE',  ( 9.855200000000998273, -3579.494999999999891, 2256.063560000000052 ) ) ;
#6701 = CARTESIAN_POINT ( 'NONE',  ( 15.41923444567002655, -3580.331984414333419, 2249.826959883762356 ) ) ;
#6702 = CARTESIAN_POINT ( 'NONE',  ( 0.000000000000000000, -3578.860000000000127, 2243.277199999999993 ) ) ;
#6703 = CARTESIAN_POINT ( 'NONE',  ( 134.2390000000000043, -3659.504999999999654, 2239.391000000000076 ) ) ;
#6704 = ORIENTED_EDGE ( 'NONE', *, *, #1364, .F. ) ;
#6705 = CARTESIAN_POINT ( 'NONE',  ( -0.7620000000000000107, -3660.140000000000327, 2247.392000000000280 ) ) ;
#6706 = EDGE_CURVE ( 'NONE', #13565, #6249, #14107, .T. ) ;
#6707 = EDGE_CURVE ( 'NONE', #21395, #12304, #15746, .T. ) ;
#6708 = DIRECTION ( 'NONE',  ( 2.336881798971000105E-14, 2.336881798971000105E-14, 1.000000000000000000 ) ) ;
#6709 = EDGE_LOOP ( 'NONE', ( #22356, #8668, #6737, #20906 ) ) ;
#6710 = VECTOR ( 'NONE', #20943, 1000.000000000000000 ) ;
#6711 = SPHERICAL_SURFACE ( 'NONE', #15838, 0.7620000000000000107 ) ;
#6712 = LINE ( 'NONE', #8579, #5078 ) ;
#6713 = VERTEX_POINT ( 'NONE', #3545 ) ;
#6714 = DIRECTION ( 'NONE',  ( 1.000000000000000000, 0.000000000000000000, 0.000000000000000000 ) ) ;
#6715 = LINE ( 'NONE', #22974, #15923 ) ;
#6716 = EDGE_CURVE ( 'NONE', #12318, #12735, #6731, .T. ) ;
#6717 = ORIENTED_EDGE ( 'NONE', *, *, #6576, .T. ) ;
#6718 = CARTESIAN_POINT ( 'NONE',  ( 9.855200000000680305, -3659.053785370519563, 2256.063559999999597 ) ) ;
#6719 = DIRECTION ( 'NONE',  ( 0.000000000000000000, 0.000000000000000000, -1.000000000000000000 ) ) ;
#6720 = DIRECTION ( 'NONE',  ( 1.000000000000000000, 5.432398939370943590E-28, -2.324635735433000369E-14 ) ) ;
#6721 = CARTESIAN_POINT ( 'NONE',  ( 12.69999999999999929, -3648.710000000000036, 2257.592639999999847 ) ) ;
#6722 = EDGE_CURVE ( 'NONE', #13045, #6818, #10232, .T. ) ;
#6723 = PERSON_AND_ORGANIZATION_ROLE ( 'design_owner' ) ;
#6724 = ADVANCED_FACE ( 'NONE', ( #6965 ), #39, .F. ) ;
#6725 = FACE_OUTER_BOUND ( 'NONE', #19973, .T. ) ;
#6726 = DIRECTION ( 'NONE',  ( 0.000000000000000000, 0.000000000000000000, -1.000000000000000000 ) ) ;
#6727 = FACE_OUTER_BOUND ( 'NONE', #14311, .T. ) ;
#6728 = TOROIDAL_SURFACE ( 'NONE', #11552, 3.606799999998999695, 0.7620000000000000107 ) ;
#6729 = CARTESIAN_POINT ( 'NONE',  ( 142.3063350412433863, -3658.362045441383543, 2249.614643222462746 ) ) ;
#6730 = VERTEX_POINT ( 'NONE', #1321 ) ;
#6731 = LINE ( 'NONE', #7079, #14479 ) ;
#6732 = EDGE_CURVE ( 'NONE', #6472, #12668, #9971, .T. ) ;
#6733 = VERTEX_POINT ( 'NONE', #12580 ) ;
#6734 = VERTEX_POINT ( 'NONE', #14221 ) ;
#6735 = CIRCLE ( 'NONE', #17573, 0.7619999999999987894 ) ;
#6736 = DIRECTION ( 'NONE',  ( 0.8660254037827048723, 0.5000000000030029312, 0.000000000000000000 ) ) ;
#6737 = ORIENTED_EDGE ( 'NONE', *, *, #5372, .T. ) ;
#6738 = ORIENTED_EDGE ( 'NONE', *, *, #21279, .F. ) ;
#6739 = SECURITY_CLASSIFICATION ( '', '', #3159 ) ;
#6740 = CARTESIAN_POINT ( 'NONE',  ( 25.39999999999999858, -3670.300000000000182, 2239.771999999999935 ) ) ;
#6741 = CYLINDRICAL_SURFACE ( 'NONE', #8038, 2.844799999999994444 ) ;
#6742 = CARTESIAN_POINT ( 'NONE',  ( 132.3005794017000198, -3544.570000000000164, 2260.390449568000349 ) ) ;
#6743 = ORIENTED_EDGE ( 'NONE', *, *, #9705, .T. ) ;
#6744 = DIRECTION ( 'NONE',  ( -1.000000000000000000, 0.000000000000000000, 0.000000000000000000 ) ) ;
#6745 = DIRECTION ( 'NONE',  ( 1.000000000000000000, 0.000000000000000000, 0.000000000000000000 ) ) ;
#6746 = FACE_OUTER_BOUND ( 'NONE', #14983, .T. ) ;
#6747 = CARTESIAN_POINT ( 'NONE',  ( 138.9614759198583727, -3656.751457182684589, 2257.615706725407563 ) ) ;
#6748 = CARTESIAN_POINT ( 'NONE',  ( -12.31900000000000084, -3660.140000000000327, 2250.104686796999886 ) ) ;
#6749 = VERTEX_POINT ( 'NONE', #5201 ) ;
#6750 = ADVANCED_FACE ( 'NONE', ( #10463 ), #21021, .T. ) ;
#6751 = PERSON_AND_ORGANIZATION ( #5446, #1895 ) ;
#6752 = ORIENTED_EDGE ( 'NONE', *, *, #11854, .T. ) ;
#6753 = DIRECTION ( 'NONE',  ( 0.000000000000000000, -1.000000000000000000, 0.000000000000000000 ) ) ;
#6754 = CIRCLE ( 'NONE', #20231, 0.7619999999999294005 ) ;
#6755 = CARTESIAN_POINT ( 'NONE',  ( 10.84069775277338010, -3581.649407856291873, 2246.804666700250891 ) ) ;
#6756 = DIRECTION ( 'NONE',  ( 0.000000000000000000, 0.000000000000000000, -1.000000000000000000 ) ) ;
#6757 = LOCAL_TIME ( 17, 37, 43.00000000000000000, #11131 ) ;
#6758 = B_SPLINE_CURVE_WITH_KNOTS ( 'NONE', 3,
 ( #7688, #14733, #21980, #7353, #20124, #5718, #13076, #10976, #4171, #14385, #11315, #21533, #12850, #3943, #2196, #1957, #18122, #203, #20007, #9226, #11098, #5602, #18465, #5489, #9340, #16475, #4057, #2418, #14505, #16706, #7574, #7237, #19779, #3706, #11205, #10860, #2080, #18010, #9112, #12734, #19889, #16366, #319, #20456, #16814, #15071 ),
 .UNSPECIFIED., .F., .F.,
 ( 4, 2, 2, 1, 2, 2, 2, 2, 1, 1, 1, 1, 2, 2, 2, 2, 2, 1, 2, 2, 2, 2, 1, 1, 2, 2, 4 ),
 ( 0.000000000000000000, 0.1250000000022165880, 0.1875000000033248126, 0.2187500000036660674, 0.2343750000038365700, 0.2500000000040070725, 0.3750000000057552296, 0.4375000000064863115, 0.4687500000069002026, 0.4843750000070696782, 0.4921875000073470119, 0.4960937500074050766, 0.4980468750074055206, 0.5000000000074059647, 0.5625000000084945384, 0.5937500000090564223, 0.6093750000094169117, 0.6171875000095971009, 0.6210937500096163078, 0.6250000000096355146, 0.6875000000104954934, 0.7187500000108046905, 0.7343750000108574261, 0.7421875000107768239, 0.7460937500105744302, 0.7500000000103719255, 1.000000000000000000 ),
 .UNSPECIFIED. ) ;
#6759 =( GEOMETRIC_REPRESENTATION_CONTEXT ( 3 ) GLOBAL_UNCERTAINTY_ASSIGNED_CONTEXT ( ( #13217 ) ) GLOBAL_UNIT_ASSIGNED_CONTEXT ( ( #18066, #12789, #16419 ) ) REPRESENTATION_CONTEXT ( 'NONE', 'WORKASPACE' ) );
#6760 = ORIENTED_EDGE ( 'NONE', *, *, #3855, .F. ) ;
#6761 = CARTESIAN_POINT ( 'NONE',  ( -6.349999999999999645, -3578.860000000000127, 2247.392000000000280 ) ) ;
#6762 = AXIS2_PLACEMENT_3D ( 'NONE', #10686, #9165, #2136 ) ;
#6763 = DIRECTION ( 'NONE',  ( 0.000000000000000000, 1.000000000000000000, 0.000000000000000000 ) ) ;
#6764 = CARTESIAN_POINT ( 'NONE',  ( 144.8796679668512297, -3661.919754677027413, 2245.172503498299648 ) ) ;
#6765 = CARTESIAN_POINT ( 'NONE',  ( 12.69999999999999929, -3653.789999999999964, 2268.705139999999574 ) ) ;
#6766 = FACE_OUTER_BOUND ( 'NONE', #8200, .T. ) ;
#6767 = APPROVAL ( #13922, 'UNKNOWN' ) ;
#6768 = CARTESIAN_POINT ( 'NONE',  ( 151.4000000000000057, -3544.570000000000164, 2239.039032635400417 ) ) ;
#6769 = VERTEX_POINT ( 'NONE', #10585 ) ;
#6770 = FACE_OUTER_BOUND ( 'NONE', #3, .T. ) ;
#6771 = CARTESIAN_POINT ( 'NONE',  ( -6.349999999999999645, -3544.061999999999898, 2229.612000000000080 ) ) ;
#6772 = DIRECTION ( 'NONE',  ( 1.000000000000000000, 4.198251155732999970E-13, 0.000000000000000000 ) ) ;
#6773 = CARTESIAN_POINT ( 'NONE',  ( 55.57575231171000496, -3694.938000000000102, 2275.763800000000174 ) ) ;
#6774 = CARTESIAN_POINT ( 'NONE',  ( 15.03168679707234467, -3600.843700000039007, 2296.210799999999836 ) ) ;
#6775 = SECURITY_CLASSIFICATION ( '', '', #20676 ) ;
#6776 = VERTEX_POINT ( 'NONE', #14343 ) ;
#6777 = AXIS2_PLACEMENT_3D ( 'NONE', #5653, #15127, #6231 ) ;
#6778 = VERTEX_POINT ( 'NONE', #4961 ) ;
#6779 = ORIENTED_EDGE ( 'NONE', *, *, #8454, .T. ) ;
#6780 = DIRECTION ( 'NONE',  ( 6.119339505807659940E-14, -1.000000000000000000, 0.000000000000000000 ) ) ;
#6781 = CALENDAR_DATE ( 2026, 26, 10 ) ;
#6782 = AXIS2_PLACEMENT_3D ( 'NONE', #22652, #3555, #14232 ) ;
#6783 = CYLINDRICAL_SURFACE ( 'NONE', #2339, 0.7619999999999996776 ) ;
#6784 = CARTESIAN_POINT ( 'NONE',  ( 10.32641459757000035, -3657.928429337000125, 2257.848701351999807 ) ) ;
#6785 = DIRECTION ( 'NONE',  ( 1.000000000000000000, 0.000000000000000000, 0.000000000000000000 ) ) ;
#6786 = CARTESIAN_POINT ( 'NONE',  ( 15.07358448401000217, -3657.928427944000305, 2257.848701151000114 ) ) ;
#6787 = CARTESIAN_POINT ( 'NONE',  ( -0.7620000000000000107, -3694.938000000000102, 2253.487999999999829 ) ) ;
#6788 = APPLICATION_CONTEXT ( 'configuration controlled 3d designs of mechanical parts and assemblies' ) ;
#6789 = LOCAL_TIME ( 17, 37, 43.00000000000000000, #3207 ) ;
#6790 = FACE_OUTER_BOUND ( 'NONE', #14550, .T. ) ;
#6791 = VERTEX_POINT ( 'NONE', #21488 ) ;
#6792 = FACE_OUTER_BOUND ( 'NONE', #7532, .T. ) ;
#6793 = APPLIED_DATE_AND_TIME_ASSIGNMENT ( #13947, #15705, ( #22959 ) ) ;
#6794 = FACE_OUTER_BOUND ( 'NONE', #19712, .T. ) ;
#6795 = EDGE_LOOP ( 'NONE', ( #15260, #1146, #13820, #15284 ) ) ;
#6796 = DIRECTION ( 'NONE',  ( 0.7249994335945011414, 6.337882393832011514E-14, -0.6887494619146010688 ) ) ;
#6797 = CARTESIAN_POINT ( 'NONE',  ( 10.83541561206130055, -3657.356279649904991, 2247.981293899261800 ) ) ;
#6798 = AXIS2_PLACEMENT_3D ( 'NONE', #10753, #5367, #90 ) ;
#6799 = AXIS2_PLACEMENT_3D ( 'NONE', #23087, #7064, #13972 ) ;
#6800 = ADVANCED_FACE ( 'NONE', ( #8488 ), #19731, .T. ) ;
#6801 = ORIENTED_EDGE ( 'NONE', *, *, #19432, .F. ) ;
#6802 = CARTESIAN_POINT ( 'NONE',  ( 132.3005794017000198, -3694.430000000000291, 2260.390449568000349 ) ) ;
#6803 = EDGE_CURVE ( 'NONE', #14462, #18372, #4236, .T. ) ;
#6804 = ORIENTED_EDGE ( 'NONE', *, *, #20754, .T. ) ;
#6805 = EDGE_CURVE ( 'NONE', #9634, #21213, #13356, .T. ) ;
#6806 = CARTESIAN_POINT ( 'NONE',  ( 95.25000000000000000, -3544.570000000000164, 2247.392000000000280 ) ) ;
#6807 = APPROVAL_DATE_TIME ( #19222, #889 ) ;
#6808 = DIRECTION ( 'NONE',  ( -1.000000000000000000, 0.000000000000000000, 0.000000000000000000 ) ) ;
#6809 = ORIENTED_EDGE ( 'NONE', *, *, #9579, .F. ) ;
#6810 = CARTESIAN_POINT ( 'NONE',  ( 137.1443557123595554, -3580.758427011661297, 2257.890254637431099 ) ) ;
#6811 = DATE_AND_TIME ( #7153, #15343 ) ;
#6812 = DIRECTION ( 'NONE',  ( -1.000000000000000000, 0.000000000000000000, 0.000000000000000000 ) ) ;
#6813 = CARTESIAN_POINT ( 'NONE',  ( 0.7620000000000000107, -3544.061999999999898, 2275.763800000000174 ) ) ;
#6814 = CARTESIAN_POINT ( 'NONE',  ( 134.0389477936680294, -3658.715683113317937, 2244.927055122274851 ) ) ;
#6815 = AXIS2_PLACEMENT_3D ( 'NONE', #17676, #1624, #15349 ) ;
#6816 = EDGE_CURVE ( 'NONE', #2094, #17500, #18855, .T. ) ;
#6817 = CARTESIAN_POINT ( 'NONE',  ( 9.855199999999999960, -3599.497499999999945, 2263.571799999999712 ) ) ;
#6818 = VERTEX_POINT ( 'NONE', #15140 ) ;
#6819 = CARTESIAN_POINT ( 'NONE',  ( 15.28726622823146819, -3695.066554908766193, 2255.655515827249928 ) ) ;
#6820 = CARTESIAN_POINT ( 'NONE',  ( -12.69999999979383887, -3575.985370510264602, 2247.391999999993459 ) ) ;
#6821 = ORIENTED_EDGE ( 'NONE', *, *, #18090, .F. ) ;
#6822 = DIRECTION ( 'NONE',  ( 1.000000000000000000, 0.000000000000000000, 0.000000000000000000 ) ) ;
#6823 = VECTOR ( 'NONE', #10956, 1000.000000000000000 ) ;
#6824 = DIRECTION ( 'NONE',  ( 0.000000000000000000, 0.000000000000000000, -1.000000000000000000 ) ) ;
#6825 = ORIENTED_EDGE ( 'NONE', *, *, #9965, .F. ) ;
#6826 = ORIENTED_EDGE ( 'NONE', *, *, #10259, .F. ) ;
#6827 = SPHERICAL_SURFACE ( 'NONE', #3050, 1.270000000000000018 ) ;
#6828 = CIRCLE ( 'NONE', #15801, 2.844800000000091700 ) ;
#6829 = DIRECTION ( 'NONE',  ( -1.000000000000000000, 0.000000000000000000, 0.000000000000000000 ) ) ;
#6830 = CIRCLE ( 'NONE', #5717, 4.114799999999974034 ) ;
#6831 = ORIENTED_EDGE ( 'NONE', *, *, #705, .F. ) ;
#6832 = EDGE_CURVE ( 'NONE', #16601, #9582, #277, .T. ) ;
#6833 = CIRCLE ( 'NONE', #3827, 3.606800000000000228 ) ;
#6834 = DIRECTION ( 'NONE',  ( 0.000000000000000000, 0.000000000000000000, -1.000000000000000000 ) ) ;
#6835 = DIRECTION ( 'NONE',  ( 1.000000000000000000, 0.000000000000000000, 0.000000000000000000 ) ) ;
#6836 = FACE_OUTER_BOUND ( 'NONE', #10328, .T. ) ;
#6837 = CARTESIAN_POINT ( 'NONE',  ( 12.69999999999999929, -3639.502500000000055, 2263.571799999999712 ) ) ;
#6838 = CALENDAR_DATE ( 2026, 26, 10 ) ;
#6839 = EDGE_CURVE ( 'NONE', #6888, #6776, #8497, .T. ) ;
#6840 = ADVANCED_FACE ( 'NONE', ( #18647 ), #6470, .T. ) ;
#6841 = FACE_OUTER_BOUND ( 'NONE', #5441, .T. ) ;
#6842 = CARTESIAN_POINT ( 'NONE',  ( 145.4149999999999920, -3659.504999999999654, 2239.771999999999935 ) ) ;
#6843 = CARTESIAN_POINT ( 'NONE',  ( 18.38430049721045023, -3580.087277414933851, 2244.825193658544322 ) ) ;
#6844 = CIRCLE ( 'NONE', #8358, 2.844799999999994444 ) ;
#6845 = CARTESIAN_POINT ( 'NONE',  ( 142.0919336763783463, -3657.965060599514345, 2249.225720191686378 ) ) ;
#6846 = ORIENTED_EDGE ( 'NONE', *, *, #20293, .F. ) ;
#6847 = AXIS2_PLACEMENT_3D ( 'NONE', #1690, #14008, #22890 ) ;
#6848 = FACE_OUTER_BOUND ( 'NONE', #11702, .T. ) ;
#6849 = CIRCLE ( 'NONE', #21079, 5.460999999999938126 ) ;
#6850 = ORIENTED_EDGE ( 'NONE', *, *, #8235, .F. ) ;
#6851 = VERTEX_POINT ( 'NONE', #22615 ) ;
#6852 = ORIENTED_EDGE ( 'NONE', *, *, #22718, .T. ) ;
#6853 = ADVANCED_FACE ( 'NONE', ( #11725 ), #22384, .T. ) ;
#6854 = FACE_OUTER_BOUND ( 'NONE', #15933, .T. ) ;
#6855 = ORIENTED_EDGE ( 'NONE', *, *, #16169, .T. ) ;
#6856 = ORIENTED_EDGE ( 'NONE', *, *, #3988, .F. ) ;
#6857 = DIRECTION ( 'NONE',  ( -2.343004830739999973E-14, -1.784212334590129905E-30, -1.000000000000000000 ) ) ;
#6858 = DATE_AND_TIME ( #5444, #21756 ) ;
#6859 = DIRECTION ( 'NONE',  ( 0.000000000000000000, -1.000000000000000000, 0.000000000000000000 ) ) ;
#6860 = CARTESIAN_POINT ( 'NONE',  ( 142.5447999999989861, -3659.504999999999654, 2257.962944264955695 ) ) ;
#6861 = VERTEX_POINT ( 'NONE', #4465 ) ;
#6862 = CYLINDRICAL_SURFACE ( 'NONE', #12955, 0.3809999999998149867 ) ;
#6863 = DIRECTION ( 'NONE',  ( 0.000000000000000000, 0.000000000000000000, -1.000000000000000000 ) ) ;
#6864 = PLANE ( 'NONE',  #10954 ) ;
#6865 = AXIS2_PLACEMENT_3D ( 'NONE', #3327, #5220, #8381 ) ;
#6866 = CARTESIAN_POINT ( 'NONE',  ( 20.34169023495000062, -3694.797466901999996, 2260.545675974999995 ) ) ;
#6867 = VERTEX_POINT ( 'NONE', #20304 ) ;
#6868 = APPLICATION_PROTOCOL_DEFINITION ( 'international standard', 'automotive_design', 2000, #15162 ) ;
#6869 = EDGE_CURVE ( 'NONE', #11706, #9059, #9855, .T. ) ;
#6870 = ORIENTED_EDGE ( 'NONE', *, *, #15737, .F. ) ;
#6871 = CYLINDRICAL_SURFACE ( 'NONE', #18753, 2.844799999999994444 ) ;
#6872 = DIRECTION ( 'NONE',  ( 0.000000000000000000, 0.000000000000000000, -1.000000000000000000 ) ) ;
#6873 = ORIENTED_EDGE ( 'NONE', *, *, #17358, .T. ) ;
#6874 = CARTESIAN_POINT ( 'NONE',  ( 127.0000000000000000, -3660.140000000000327, 2247.392000000000280 ) ) ;
#6875 = VERTEX_POINT ( 'NONE', #16995 ) ;
#6876 = AXIS2_PLACEMENT_3D ( 'NONE', #7161, #12545, #10785 ) ;
#6877 = CARTESIAN_POINT ( 'NONE',  ( 25.39999999999999858, -3619.500000000000000, 2239.009999999999764 ) ) ;
#6878 = CIRCLE ( 'NONE', #12101, 0.7619999999999987894 ) ;
#6879 = FACE_OUTER_BOUND ( 'NONE', #7974, .T. ) ;
#6880 = CARTESIAN_POINT ( 'NONE',  ( 145.3795747169000094, -3578.859731361000286, 2244.547525601999951 ) ) ;
#6881 = EDGE_CURVE ( 'NONE', #2597, #15615, #7388, .T. ) ;
#6882 = CIRCLE ( 'NONE', #18782, 11.11249999999999716 ) ;
#6883 = DIRECTION ( 'NONE',  ( 0.000000000000000000, -1.000000000000000000, 0.000000000000000000 ) ) ;
#6884 = ADVANCED_FACE ( 'NONE', ( #15031 ), #8339, .F. ) ;
#6885 = CARTESIAN_POINT ( 'NONE',  ( 11.35172555707717379, -3662.010415283757993, 2249.535724915129322 ) ) ;
#6886 = AXIS2_PLACEMENT_3D ( 'NONE', #6912, #14377, #11699 ) ;
#6887 = CARTESIAN_POINT ( 'NONE',  ( 139.7000000002929596, -3576.362659094888386, 2239.009999999999764 ) ) ;
#6888 = VERTEX_POINT ( 'NONE', #15482 ) ;
#6889 = CARTESIAN_POINT ( 'NONE',  ( 12.69999999999999929, -3639.502500000000055, 2263.571799999999712 ) ) ;
#6890 = CARTESIAN_POINT ( 'NONE',  ( 25.39999999999999858, -3670.300000000000182, 2260.600000000000364 ) ) ;
#6891 = CARTESIAN_POINT ( 'NONE',  ( 133.9850000019999925, -3579.494756921999851, 2244.617465693000213 ) ) ;
#6892 = CARTESIAN_POINT ( 'NONE',  ( 15.36939286637828239, -3658.521437840668568, 2249.731612551223861 ) ) ;
#6893 = DIRECTION ( 'NONE',  ( 0.000000000000000000, 0.000000000000000000, -1.000000000000000000 ) ) ;
#6894 = AXIS2_PLACEMENT_3D ( 'NONE', #3632, #8572, #8683 ) ;
#6895 = ORIENTED_EDGE ( 'NONE', *, *, #19465, .F. ) ;
#6896 = DIRECTION ( 'NONE',  ( 0.000000000000000000, 0.000000000000000000, -1.000000000000000000 ) ) ;
#6897 = EDGE_LOOP ( 'NONE', ( #17896, #680, #20630, #14488 ) ) ;
#6898 = CARTESIAN_POINT ( 'NONE',  ( 14.03509158661000100, -3582.012285900999814, 2257.672186979000344 ) ) ;
#6899 = SECURITY_CLASSIFICATION_LEVEL ( 'unclassified' ) ;
#6900 = CYLINDRICAL_SURFACE ( 'NONE', #10570, 2.844799999998995244 ) ;
#6901 = CARTESIAN_POINT ( 'NONE',  ( 139.6999999999999886, -3579.494999999999891, 2246.630000000000109 ) ) ;
#6902 = DIRECTION ( 'NONE',  ( 0.000000000000000000, 0.000000000000000000, 1.000000000000000000 ) ) ;
#6903 = DIRECTION ( 'NONE',  ( -0.6887494619146540265, 0.000000000000000000, -0.7249994335944508483 ) ) ;
#6904 = CARTESIAN_POINT ( 'NONE',  ( 17.45971744210237020, -3576.330750010172778, 2246.087203520595722 ) ) ;
#6905 = CARTESIAN_POINT ( 'NONE',  ( 10.36831320285999958, -3580.841199999999844, 2242.820000000000164 ) ) ;
#6906 = ORIENTED_EDGE ( 'NONE', *, *, #8942, .T. ) ;
#6907 = AXIS2_PLACEMENT_3D ( 'NONE', #10555, #3514, #1291 ) ;
#6908 = CARTESIAN_POINT ( 'NONE',  ( -6.730999999999880856, -3578.860000000000127, 2252.472000000000207 ) ) ;
#6909 = DIRECTION ( 'NONE',  ( -3.106212348370000105E-13, -6.475491540576999783E-13, 1.000000000000000000 ) ) ;
#6910 = ORIENTED_EDGE ( 'NONE', *, *, #21012, .F. ) ;
#6911 = CARTESIAN_POINT ( 'NONE',  ( 151.1299999999999955, -3544.570000000000164, 2240.279999999999745 ) ) ;
#6912 = CARTESIAN_POINT ( 'NONE',  ( 25.39999999999999858, -3619.500000000000000, 2259.837999999999738 ) ) ;
#6913 = ORIENTED_EDGE ( 'NONE', *, *, #7130, .T. ) ;
#6914 = CARTESIAN_POINT ( 'NONE',  ( 134.3329781701244485, -3581.459545042529953, 2246.234697007345403 ) ) ;
#6915 = ORIENTED_EDGE ( 'NONE', *, *, #7235, .F. ) ;
#6916 = FACE_BOUND ( 'NONE', #14347, .T. ) ;
#6917 = COORDINATED_UNIVERSAL_TIME_OFFSET ( 0, 0, .AHEAD. ) ;
#6918 = FACE_OUTER_BOUND ( 'NONE', #17028, .T. ) ;
#6919 = ORIENTED_EDGE ( 'NONE', *, *, #20017, .T. ) ;
#6920 = FACE_OUTER_BOUND ( 'NONE', #3156, .T. ) ;
#6921 = AXIS2_PLACEMENT_3D ( 'NONE', #6531, #12025, #3111 ) ;
#6922 = CALENDAR_DATE ( 2026, 26, 10 ) ;
#6923 = APPLIED_PERSON_AND_ORGANIZATION_ASSIGNMENT ( #22177, #21847, ( #21176 ) ) ;
#6924 = AXIS2_PLACEMENT_3D ( 'NONE', #20543, #2293, #11303 ) ;
#6925 = EDGE_CURVE ( 'NONE', #3332, #22999, #2595, .T. ) ;
#6926 = DIRECTION ( 'NONE',  ( 0.000000000000000000, 0.000000000000000000, -1.000000000000000000 ) ) ;
#6927 = CARTESIAN_POINT ( 'NONE',  ( 15.54480025890283912, -3579.679221764684371, 2250.122839540403220 ) ) ;
#6928 = CARTESIAN_POINT ( 'NONE',  ( 136.9873132028999976, -3579.494999999999891, 2239.391000000000076 ) ) ;
#6929 = CARTESIAN_POINT ( 'NONE',  ( 151.1299999999999955, -3544.570000000000164, 2260.600000000000364 ) ) ;
#6930 = EDGE_CURVE ( 'NONE', #14398, #15285, #11605, .T. ) ;
#6931 = ADVANCED_FACE ( 'NONE', ( #11384 ), #20518, .T. ) ;
#6932 = CARTESIAN_POINT ( 'NONE',  ( -12.31900000000012874, -3578.860000000000127, 2241.931000000000040 ) ) ;
#6933 = ORIENTED_EDGE ( 'NONE', *, *, #2131, .T. ) ;
#6934 = CARTESIAN_POINT ( 'NONE',  ( 12.69999999999999929, -3648.710000000000036, 2261.593139999999948 ) ) ;
#6935 = EDGE_CURVE ( 'NONE', #12473, #12697, #12174, .T. ) ;
#6936 = CARTESIAN_POINT ( 'NONE',  ( 15.21772229205999949, -3578.160722075999729, 2257.881333375999930 ) ) ;
#6937 = ORIENTED_EDGE ( 'NONE', *, *, #23112, .T. ) ;
#6938 = VECTOR ( 'NONE', #2599, 1000.000000000000000 ) ;
#6939 = DIRECTION ( 'NONE',  ( 0.000000000000000000, 0.000000000000000000, 1.000000000000000000 ) ) ;
#6940 = TOROIDAL_SURFACE ( 'NONE', #13277, 3.606799999999999784, 0.7620000000000000107 ) ;
#6941 = AXIS2_PLACEMENT_3D ( 'NONE', #5620, #21666, #12644 ) ;
#6942 = CARTESIAN_POINT ( 'NONE',  ( 21.79320000000099711, -3670.300000000000182, 2260.600000000000364 ) ) ;
#6943 = VECTOR ( 'NONE', #14667, 1000.000000000000000 ) ;
#6944 = VERTEX_POINT ( 'NONE', #7993 ) ;
#6945 = EDGE_CURVE ( 'NONE', #21023, #16784, #17408, .T. ) ;
#6946 = EDGE_LOOP ( 'NONE', ( #9523, #22595, #12694, #3543 ) ) ;
#6947 = CARTESIAN_POINT ( 'NONE',  ( 64.76999999999999602, -3670.300000000000182, 2292.057900000000245 ) ) ;
#6948 = ORIENTED_EDGE ( 'NONE', *, *, #15136, .T. ) ;
#6949 = LINE ( 'NONE', #17478, #9821 ) ;
#6950 = DIRECTION ( 'NONE',  ( 0.000000000000000000, 0.000000000000000000, -1.000000000000000000 ) ) ;
#6951 = DIRECTION ( 'NONE',  ( -0.000000000000000000, -1.000000000000000000, -0.000000000000000000 ) ) ;
#6952 = EDGE_CURVE ( 'NONE', #9982, #4022, #16306, .T. ) ;
#6953 = DIRECTION ( 'NONE',  ( -1.752935795934731214E-12, -1.000000000000000000, -1.748382715945290473E-12 ) ) ;
#6954 = DATE_AND_TIME ( #10455, #14231 ) ;
#6955 = DIRECTION ( 'NONE',  ( -1.000000000000000000, 0.000000000000000000, 0.000000000000000000 ) ) ;
#6956 = CARTESIAN_POINT ( 'NONE',  ( 10.01182667074545840, -3695.327183877031530, 2255.402926848606057 ) ) ;
#6957 = CYLINDRICAL_SURFACE ( 'NONE', #2192, 0.3810000000000260956 ) ;
#6958 = VECTOR ( 'NONE', #2409, 1000.000000000000000 ) ;
#6959 = PRODUCT ( 'Screw 3', 'Screw 3', '', ( #16676 ) ) ;
#6960 = CARTESIAN_POINT ( 'NONE',  ( 137.3255051320594475, -3657.938320579140509, 2249.193689002128849 ) ) ;
#6961 = AXIS2_PLACEMENT_3D ( 'NONE', #22332, #16944, #2546 ) ;
#6962 = ORIENTED_EDGE ( 'NONE', *, *, #634, .T. ) ;
#6963 = AXIS2_PLACEMENT_3D ( 'NONE', #22267, #7878, #6245 ) ;
#6964 = ADVANCED_FACE ( 'NONE', ( #12429 ), #6205, .T. ) ;
#6965 = FACE_OUTER_BOUND ( 'NONE', #8081, .T. ) ;
#6966 = EDGE_CURVE ( 'NONE', #1715, #12697, #4813, .T. ) ;
#6967 = ORIENTED_EDGE ( 'NONE', *, *, #21178, .F. ) ;
#6968 = AXIS2_PLACEMENT_3D ( 'NONE', #12221, #22400, #3307 ) ;
#6969 = ORIENTED_EDGE ( 'NONE', *, *, #7361, .F. ) ;
#6970 = ORIENTED_EDGE ( 'NONE', *, *, #6250, .F. ) ;
#6971 = LINE ( 'NONE', #1680, #20812 ) ;
#6972 = ORIENTED_EDGE ( 'NONE', *, *, #22811, .T. ) ;
#6973 = ORIENTED_EDGE ( 'NONE', *, *, #3222, .F. ) ;
#6974 = CARTESIAN_POINT ( 'NONE',  ( 142.5448000000000093, -3659.504999999999654, 2256.063560000000052 ) ) ;
#6975 = AXIS2_PLACEMENT_3D ( 'NONE', #6509, #20667, #20790 ) ;
#6976 = PERSON_AND_ORGANIZATION ( #14121, #20619 ) ;
#6977 = DIRECTION ( 'NONE',  ( 1.000000000000000000, 0.000000000000000000, 0.000000000000000000 ) ) ;
#6978 = AXIS2_PLACEMENT_3D ( 'NONE', #17642, #3465, #1592 ) ;
#6979 = CARTESIAN_POINT ( 'NONE',  ( 136.8551999999999964, -3659.504999999999654, 2256.063560000000052 ) ) ;
#6980 = ORIENTED_EDGE ( 'NONE', *, *, #11576, .F. ) ;
#6981 = AXIS2_PLACEMENT_3D ( 'NONE', #5979, #11465, #20596 ) ;
#6982 = CARTESIAN_POINT ( 'NONE',  ( 136.8552000000001669, -3579.946214629432689, 2256.063560000000052 ) ) ;
#6983 = FACE_BOUND ( 'NONE', #13974, .T. ) ;
#6984 = CYLINDRICAL_SURFACE ( 'NONE', #5357, 0.7619999999999230722 ) ;
#6985 = SHAPE_REPRESENTATION ( 'Hinge 1', ( #5611 ), #14218 ) ;
#6986 = DIRECTION ( 'NONE',  ( 0.000000000000000000, 0.000000000000000000, -1.000000000000000000 ) ) ;
#6987 = CIRCLE ( 'NONE', #16716, 0.7619999999999294005 ) ;
#6988 = EDGE_LOOP ( 'NONE', ( #5879, #13488 ) ) ;
#6989 = COORDINATED_UNIVERSAL_TIME_OFFSET ( 0, 0, .AHEAD. ) ;
#6990 = EDGE_LOOP ( 'NONE', ( #16800, #14570, #3223, #8322 ) ) ;
#6991 = FACE_OUTER_BOUND ( 'NONE', #18654, .T. ) ;
#6992 = CARTESIAN_POINT ( 'NONE',  ( 10.73432012640060584, -3581.551840941039700, 2248.313564088525254 ) ) ;
#6993 = DIRECTION ( 'NONE',  ( 0.000000000000000000, 0.000000000000000000, -1.000000000000000000 ) ) ;
#6994 = EDGE_LOOP ( 'NONE', ( #4250, #22819, #16162, #7187, #14132, #16639 ) ) ;
#6995 = FACE_OUTER_BOUND ( 'NONE', #4130, .T. ) ;
#6996 = VECTOR ( 'NONE', #21384, 1000.000000000000000 ) ;
#6997 = DIRECTION ( 'NONE',  ( 0.5000000000048030468, 0.8660254037816655925, 0.000000000000000000 ) ) ;
#6998 = CARTESIAN_POINT ( 'NONE',  ( 144.5542768966436711, -3576.478798223026388, 2245.835328353847217 ) ) ;
#6999 = AXIS2_PLACEMENT_3D ( 'NONE', #9375, #20158, #3983 ) ;
#7000 = CARTESIAN_POINT ( 'NONE',  ( 116.8400000000000034, -3544.570000000000164, 2247.392000000000280 ) ) ;
#7001 = AXIS2_PLACEMENT_3D ( 'NONE', #9877, #8597, #13871 ) ;
#7002 = CARTESIAN_POINT ( 'NONE',  ( 11.38813178685436256, -3662.029528285001106, 2249.518792719746671 ) ) ;
#7003 = EDGE_CURVE ( 'NONE', #16212, #10141, #12134, .T. ) ;
#7004 = EDGE_CURVE ( 'NONE', #17967, #2858, #7707, .T. ) ;
#7005 = DIRECTION ( 'NONE',  ( 0.000000000000000000, 1.000000000000000000, 0.000000000000000000 ) ) ;
#7006 = VECTOR ( 'NONE', #4304, 1000.000000000000000 ) ;
#7007 = ORIENTED_EDGE ( 'NONE', *, *, #21990, .T. ) ;
#7008 = ADVANCED_FACE ( 'NONE', ( #3404 ), #20992, .F. ) ;
#7009 = DIRECTION ( 'NONE',  ( 1.000000000000000000, 0.000000000000000000, 0.000000000000000000 ) ) ;
#7010 = PLANE ( 'NONE',  #1707 ) ;
#7011 = CARTESIAN_POINT ( 'NONE',  ( 141.6126943346999951, -3657.399161235000520, 2246.630000000000109 ) ) ;
#7012 = CARTESIAN_POINT ( 'NONE',  ( 14.88809329571305540, -3657.686607509436271, 2248.833042055603983 ) ) ;
#7013 = CARTESIAN_POINT ( 'NONE',  ( 137.1293686148364372, -3694.866442831601034, 2255.697303097024360 ) ) ;
#7014 = ORIENTED_EDGE ( 'NONE', *, *, #22875, .F. ) ;
#7015 = EDGE_CURVE ( 'NONE', #5417, #12899, #12190, .T. ) ;
#7016 = CIRCLE ( 'NONE', #4753, 3.606800000000021100 ) ;
#7017 = CARTESIAN_POINT ( 'NONE',  ( 10.58927397074967125, -3577.587572210373310, 2249.936439182378308 ) ) ;
#7018 = ORIENTED_EDGE ( 'NONE', *, *, #18653, .F. ) ;
#7019 = LINE ( 'NONE', #15559, #13186 ) ;
#7020 = AXIS2_PLACEMENT_3D ( 'NONE', #21657, #9122, #5376 ) ;
#7021 = DIRECTION ( 'NONE',  ( -1.000000000000000000, 0.000000000000000000, 0.000000000000000000 ) ) ;
#7022 = DATE_AND_TIME ( #6781, #3759 ) ;
#7023 = EDGE_CURVE ( 'NONE', #5223, #6224, #10322, .T. ) ;
#7024 = ADVANCED_FACE ( 'NONE', ( #3516 ), #21343, .T. ) ;
#7025 = CARTESIAN_POINT ( 'NONE',  ( 12.60791899384999937, -3656.660200000000259, 2257.592639999999847 ) ) ;
#7026 = CARTESIAN_POINT ( 'NONE',  ( 137.7875023037999824, -3581.600928630999988, 2246.630000000000109 ) ) ;
#7027 = VERTEX_POINT ( 'NONE', #6934 ) ;
#7028 = DIRECTION ( 'NONE',  ( -1.224646799141892071E-16, -1.000000000000000000, 2.336881798971000421E-14 ) ) ;
#7029 = DIRECTION ( 'NONE',  ( -0.8928571428573600643, 0.4503400076038009403, 0.000000000000000000 ) ) ;
#7030 = DIRECTION ( 'NONE',  ( 1.000000000000000000, 0.000000000000000000, 0.000000000000000000 ) ) ;
#7031 = ORIENTED_EDGE ( 'NONE', *, *, #2566, .F. ) ;
#7032 = DIRECTION ( 'NONE',  ( 1.710167014410999932E-12, -1.000000000000000000, 0.000000000000000000 ) ) ;
#7033 = CIRCLE ( 'NONE', #23091, 1.269999999999882334 ) ;
#7034 = EDGE_CURVE ( 'NONE', #12115, #19405, #19691, .T. ) ;
#7035 = CARTESIAN_POINT ( 'NONE',  ( 35.56000000000000227, -3694.430000000000291, 2244.547199999999975 ) ) ;
#7036 = ORIENTED_EDGE ( 'NONE', *, *, #13147, .F. ) ;
#7037 = DIRECTION ( 'NONE',  ( 0.000000000000000000, 0.000000000000000000, -1.000000000000000000 ) ) ;
#7038 = VECTOR ( 'NONE', #16603, 1000.000000000000000 ) ;
#7039 = AXIS2_PLACEMENT_3D ( 'NONE', #5195, #14335, #3425 ) ;
#7040 = ORIENTED_EDGE ( 'NONE', *, *, #8524, .T. ) ;
#7041 = CARTESIAN_POINT ( 'NONE',  ( 142.2650752003752075, -3694.826579461697293, 2255.711168198594351 ) ) ;
#7042 = CARTESIAN_POINT ( 'NONE',  ( 142.5354141679999884, -3659.800641111999539, 2250.222551630000453 ) ) ;
#7043 = VERTEX_POINT ( 'NONE', #21231 ) ;
#7044 = DIRECTION ( 'NONE',  ( -1.224646799147353207E-16, 1.000000000000000000, 0.000000000000000000 ) ) ;
#7045 = EDGE_LOOP ( 'NONE', ( #12444, #12465 ) ) ;
#7046 = CARTESIAN_POINT ( 'NONE',  ( 135.0886139726999886, -3576.119152860999748, 2246.630000000000109 ) ) ;
#7047 = PERSON_AND_ORGANIZATION ( #5446, #1895 ) ;
#7048 = CIRCLE ( 'NONE', #20883, 6.349999999999855760 ) ;
#7049 = CARTESIAN_POINT ( 'NONE',  ( 15.54479999999999862, -3659.504999999999654, 2256.063560000000052 ) ) ;
#7050 = CARTESIAN_POINT ( 'NONE',  ( 14.87406578659674494, -3581.330107240630696, 2248.804283326418044 ) ) ;
#7051 = CARTESIAN_POINT ( 'NONE',  ( 7.238999999999998991, -3579.494999999999891, 2239.391000000000531 ) ) ;
#7052 = AXIS2_PLACEMENT_3D ( 'NONE', #13168, #1638, #12543 ) ;
#7053 = CARTESIAN_POINT ( 'NONE',  ( 15.54479999999999862, -3639.502500000000055, 2281.351799999999912 ) ) ;
#7054 = DIRECTION ( 'NONE',  ( -0.8660254037817188832, 0.5000000000047110094, 0.000000000000000000 ) ) ;
#7055 = ORIENTED_EDGE ( 'NONE', *, *, #21693, .T. ) ;
#7056 = CARTESIAN_POINT ( 'NONE',  ( 15.38582118512052510, -3695.321318630521546, 2255.408746714442714 ) ) ;
#7057 = ORIENTED_EDGE ( 'NONE', *, *, #18375, .T. ) ;
#7058 = CARTESIAN_POINT ( 'NONE',  ( 12.69999999999999929, -3579.494999999999891, 2246.630000000000109 ) ) ;
#7059 = CARTESIAN_POINT ( 'NONE',  ( 136.8551999999999964, -3659.504999999999654, 2256.063560000000052 ) ) ;
#7060 = APPLIED_DATE_AND_TIME_ASSIGNMENT ( #6091, #16744, ( #13118 ) ) ;
#7061 = AXIS2_PLACEMENT_3D ( 'NONE', #21133, #19605, #4954 ) ;
#7062 = FACE_OUTER_BOUND ( 'NONE', #17925, .T. ) ;
#7063 = EDGE_LOOP ( 'NONE', ( #21649, #22784, #10417, #7369, #15537, #3881 ) ) ;
#7064 = DIRECTION ( 'NONE',  ( 0.000000000000000000, 1.000000000000000000, 0.000000000000000000 ) ) ;
#7065 = DIRECTION ( 'NONE',  ( -1.000000000000000000, 0.000000000000000000, 0.000000000000000000 ) ) ;
#7066 = VERTEX_POINT ( 'NONE', #13959 ) ;
#7067 = DIRECTION ( 'NONE',  ( 0.8068916933301631955, -0.5906994119133536225, 0.000000000000000000 ) ) ;
#7068 = FACE_OUTER_BOUND ( 'NONE', #6154, .T. ) ;
#7069 = EDGE_CURVE ( 'NONE', #22409, #11834, #22644, .T. ) ;
#7070 = CARTESIAN_POINT ( 'NONE',  ( 1.270000000000000018, -3544.570000000000164, 2260.600000000000364 ) ) ;
#7071 = DATE_AND_TIME ( #5307, #11 ) ;
#7072 = EDGE_CURVE ( 'NONE', #18510, #5531, #23034, .T. ) ;
#7073 = CARTESIAN_POINT ( 'NONE',  ( 12.69999999999133955, -3642.194900000167763, 2296.433984632682041 ) ) ;
#7074 = CARTESIAN_POINT ( 'NONE',  ( 10.00637276908404161, -3695.340677396607134, 2255.389249077402383 ) ) ;
#7075 = CARTESIAN_POINT ( 'NONE',  ( 7.238999999999998991, -3659.504999999999654, 2239.391000000000531 ) ) ;
#7076 = CARTESIAN_POINT ( 'NONE',  ( 137.6322476998775244, -3657.550994620480651, 2248.571276128920090 ) ) ;
#7077 = ORIENTED_EDGE ( 'NONE', *, *, #3420, .F. ) ;
#7078 = AXIS2_PLACEMENT_3D ( 'NONE', #16163, #21893, #14756 ) ;
#7079 = CARTESIAN_POINT ( 'NONE',  ( 15.54479999999999862, -3599.497499999999945, 2263.571799999999712 ) ) ;
#7080 = EDGE_LOOP ( 'NONE', ( #7847, #9604, #20855, #21388 ) ) ;
#7081 = EDGE_LOOP ( 'NONE', ( #8950, #17446, #19795, #11793 ) ) ;
#7082 = VERTEX_POINT ( 'NONE', #16406 ) ;
#7083 = APPLIED_DATE_AND_TIME_ASSIGNMENT ( #16477, #16251, ( #17087 ) ) ;
#7084 = LINE ( 'NONE', #1915, #19277 ) ;
#7085 = ORIENTED_EDGE ( 'NONE', *, *, #20679, .T. ) ;
#7086 = VERTEX_POINT ( 'NONE', #9270 ) ;
#7087 = LINE ( 'NONE', #15987, #5289 ) ;
#7088 = CARTESIAN_POINT ( 'NONE',  ( -0.7620000000000000107, -3694.938000000000102, 2253.487999999999829 ) ) ;
#7089 = DIRECTION ( 'NONE',  ( 0.000000000000000000, 0.000000000000000000, -1.000000000000000000 ) ) ;
#7090 = ORIENTED_EDGE ( 'NONE', *, *, #4131, .F. ) ;
#7091 = CARTESIAN_POINT ( 'NONE',  ( 0.000000000000000000, -3544.061999999999898, 2275.763800000000174 ) ) ;
#7092 = EDGE_CURVE ( 'NONE', #14242, #2427, #5085, .T. ) ;
#7093 = FACE_BOUND ( 'NONE', #1675, .T. ) ;
#7094 = TOROIDAL_SURFACE ( 'NONE', #347, 3.606799999999999784, 0.7620000000000000107 ) ;
#7095 = CARTESIAN_POINT ( 'NONE',  ( 139.7000000001000046, -3656.812599999999748, 2242.820000000000164 ) ) ;
#7096 = ORIENTED_EDGE ( 'NONE', *, *, #2924, .T. ) ;
#7097 = PERSON_AND_ORGANIZATION ( #5446, #1895 ) ;
#7098 = EDGE_CURVE ( 'NONE', #6749, #9068, #2345, .T. ) ;
#7099 = ORIENTED_EDGE ( 'NONE', *, *, #15978, .T. ) ;
#7100 = CARTESIAN_POINT ( 'NONE',  ( -12.69999999999998153, -3658.573829547082369, 2250.104686796773422 ) ) ;
#7101 = CARTESIAN_POINT ( 'NONE',  ( 0.000000000000000000, -3578.860000000000127, 2247.392000000000280 ) ) ;
#7102 = CARTESIAN_POINT ( 'NONE',  ( 38.10000000000000142, -3594.099999999999909, 2260.600000000000364 ) ) ;
#7103 = VERTEX_POINT ( 'NONE', #19814 ) ;
#7104 = DIRECTION ( 'NONE',  ( 1.224646799141920914E-16, -1.000000000000000000, -2.336881798971000421E-14 ) ) ;
#7105 = LOCAL_TIME ( 17, 37, 43.00000000000000000, #13979 ) ;
#7106 = EDGE_CURVE ( 'NONE', #9540, #12400, #11066, .T. ) ;
#7107 = CARTESIAN_POINT ( 'NONE',  ( 10.21049783566652813, -3578.057685255121214, 2239.010000000076616 ) ) ;
#7108 = FACE_BOUND ( 'NONE', #1988, .T. ) ;
#7109 = AXIS2_PLACEMENT_3D ( 'NONE', #15294, #11894, #17507 ) ;
#7110 = CARTESIAN_POINT ( 'NONE',  ( 131.7757523116999891, -3694.430000000000291, 2260.600000000000364 ) ) ;
#7111 = DIRECTION ( 'NONE',  ( 0.6887494619136477203, 0.000000000000000000, -0.7249994335954068614 ) ) ;
#7112 = CARTESIAN_POINT ( 'NONE',  ( 15.54478274857000031, -3659.508323119057422, 2250.165783369506698 ) ) ;
#7113 = EDGE_LOOP ( 'NONE', ( #13730, #15749, #22251, #311 ) ) ;
#7114 = FACE_OUTER_BOUND ( 'NONE', #10937, .T. ) ;
#7115 = DIRECTION ( 'NONE',  ( 1.000000000000000000, 0.000000000000000000, 0.000000000000000000 ) ) ;
#7116 = DIRECTION ( 'NONE',  ( 0.000000000000000000, 0.000000000000000000, -1.000000000000000000 ) ) ;
#7117 = CARTESIAN_POINT ( 'NONE',  ( 15.29891559246383359, -3658.345264832731573, 2249.601063626551877 ) ) ;
#7118 = CARTESIAN_POINT ( 'NONE',  ( 6.222999999999998977, -3659.504999999999654, 2239.009999999999764 ) ) ;
#7119 = ORIENTED_EDGE ( 'NONE', *, *, #12108, .T. ) ;
#7120 = CARTESIAN_POINT ( 'NONE',  ( 47.95519999999999783, -3619.500000000000000, 2261.869999999999891 ) ) ;
#7121 = VERTEX_POINT ( 'NONE', #17926 ) ;
#7122 = ADVANCED_FACE ( 'NONE', ( #13548, #4762 ), #4999, .T. ) ;
#7123 = DIRECTION ( 'NONE',  ( 0.000000000000000000, -1.000000000000000000, -2.848874176402999842E-12 ) ) ;
#7124 = LOCAL_TIME ( 17, 37, 43.00000000000000000, #14449 ) ;
#7125 = AXIS2_PLACEMENT_3D ( 'NONE', #15245, #8448, #2583 ) ;
#7126 = DIRECTION ( 'NONE',  ( -0.7249994335944036639, 0.000000000000000000, -0.6887494619147036534 ) ) ;
#7127 = CALENDAR_DATE ( 2026, 26, 10 ) ;
#7128 = EDGE_CURVE ( 'NONE', #4922, #13263, #14087, .T. ) ;
#7129 = DIRECTION ( 'NONE',  ( 1.736749921369999674E-12, -1.000000000000000000, 0.000000000000000000 ) ) ;
#7130 = EDGE_CURVE ( 'NONE', #14558, #1923, #109, .T. ) ;
#7131 = DIRECTION ( 'NONE',  ( 1.000000000000000000, 0.000000000000000000, 0.000000000000000000 ) ) ;
#7132 = CARTESIAN_POINT ( 'NONE',  ( 12.69999999999999929, -3599.497499999999945, 2281.351799999999912 ) ) ;
#7133 = CARTESIAN_POINT ( 'NONE',  ( 88.90000000000000568, -3594.099999999999909, 2239.771999999999935 ) ) ;
#7134 = DIRECTION ( 'NONE',  ( 0.000000000000000000, 0.000000000000000000, -1.000000000000000000 ) ) ;
#7135 = ORIENTED_EDGE ( 'NONE', *, *, #14104, .F. ) ;
#7136 = CYLINDRICAL_SURFACE ( 'NONE', #3585, 11.11249999999985860 ) ;
#7137 = DIRECTION ( 'NONE',  ( -2.343004830739999973E-14, -1.784212334590129905E-30, -1.000000000000000000 ) ) ;
#7138 = EDGE_LOOP ( 'NONE', ( #4656, #9586, #11733, #457 ) ) ;
#7139 = LOCAL_TIME ( 17, 37, 43.00000000000000000, #11463 ) ;
#7140 = LINE ( 'NONE', #16044, #14048 ) ;
#7141 = APPLIED_APPROVAL_ASSIGNMENT ( #4352, ( #4495 ) ) ;
#7142 = EDGE_CURVE ( 'NONE', #3607, #15456, #12139, .T. ) ;
#7143 = ORIENTED_EDGE ( 'NONE', *, *, #6288, .T. ) ;
#7144 = PLANE ( 'NONE',  #7078 ) ;
#7145 = DIRECTION ( 'NONE',  ( 0.000000000000000000, 0.000000000000000000, 1.000000000000000000 ) ) ;
#7146 = B_SPLINE_CURVE_WITH_KNOTS ( 'NONE', 3,
 ( #1127, #13799, #6662, #10272 ),
 .UNSPECIFIED., .F., .F.,
 ( 4, 4 ),
 ( 0.000000000000000000, 1.000000000000000000 ),
 .UNSPECIFIED. ) ;
#7147 = ORIENTED_EDGE ( 'NONE', *, *, #20057, .F. ) ;
#7148 = VERTEX_POINT ( 'NONE', #14145 ) ;
#7149 = PRODUCT ( 'Hinge 2', 'Hinge 2', '', ( #22607 ) ) ;
#7150 = CARTESIAN_POINT ( 'NONE',  ( 137.2652732970130103, -3580.966343291408975, 2249.304226862355335 ) ) ;
#7151 = ORIENTED_EDGE ( 'NONE', *, *, #6061, .F. ) ;
#7152 = CARTESIAN_POINT ( 'NONE',  ( 15.18950216449525925, -3658.067685255041397, 2239.009999999928368 ) ) ;
#7153 = CALENDAR_DATE ( 2026, 26, 10 ) ;
#7154 = EDGE_CURVE ( 'NONE', #1906, #20621, #18808, .T. ) ;
#7155 = DIRECTION ( 'NONE',  ( 0.000000000000000000, 0.000000000000000000, 1.000000000000000000 ) ) ;
#7156 = LOCAL_TIME ( 17, 37, 43.00000000000000000, #17777 ) ;
#7157 = DIRECTION ( 'NONE',  ( -1.000000000000000000, 0.000000000000000000, 2.324635735433000053E-14 ) ) ;
#7158 = LOCAL_TIME ( 17, 37, 43.00000000000000000, #2611 ) ;
#7159 = DIRECTION ( 'NONE',  ( 0.000000000000000000, 0.000000000000000000, -1.000000000000000000 ) ) ;
#7160 = DIRECTION ( 'NONE',  ( -1.000000000000000000, 0.000000000000000000, 0.000000000000000000 ) ) ;
#7161 = CARTESIAN_POINT ( 'NONE',  ( 50.79999999999999716, -3568.700000000000273, 2260.600000000000364 ) ) ;
#7162 = ORIENTED_EDGE ( 'NONE', *, *, #2549, .T. ) ;
#7163 = CARTESIAN_POINT ( 'NONE',  ( 134.2038178129721757, -3577.928751811623897, 2244.703885868194902 ) ) ;
#7164 = VECTOR ( 'NONE', #15063, 1000.000000000000000 ) ;
#7165 = CARTESIAN_POINT ( 'NONE',  ( 64.76999999999999602, -3544.061999999999898, 2292.057900000000245 ) ) ;
#7166 = ORIENTED_EDGE ( 'NONE', *, *, #22299, .T. ) ;
#7167 = DIRECTION ( 'NONE',  ( 1.000000000000000000, 0.000000000000000000, 0.000000000000000000 ) ) ;
#7168 = DIRECTION ( 'NONE',  ( 0.000000000000000000, 0.000000000000000000, -1.000000000000000000 ) ) ;
#7169 = EDGE_CURVE ( 'NONE', #946, #4653, #22293, .T. ) ;
#7170 = DIRECTION ( 'NONE',  ( 0.000000000000000000, 0.000000000000000000, 1.000000000000000000 ) ) ;
#7171 = VERTEX_POINT ( 'NONE', #21171 ) ;
#7172 = DIRECTION ( 'NONE',  ( 0.000000000000000000, 0.000000000000000000, -1.000000000000000000 ) ) ;
#7173 = CARTESIAN_POINT ( 'NONE',  ( 12.70000000028313281, -3656.372659094870869, 2239.009999999999764 ) ) ;
#7174 = VERTEX_POINT ( 'NONE', #12490 ) ;
#7175 = CARTESIAN_POINT ( 'NONE',  ( -6.349999999999999645, -3578.860000000000127, 2247.392000000000280 ) ) ;
#7176 = DIRECTION ( 'NONE',  ( 0.000000000000000000, 0.000000000000000000, -1.000000000000000000 ) ) ;
#7177 = CARTESIAN_POINT ( 'NONE',  ( 35.56000000000032202, -3670.300000000000182, 2244.547199999999975 ) ) ;
#7179 = CARTESIAN_POINT ( 'NONE',  ( 38.10000000000000142, -3644.899999999999636, 2261.869999999999891 ) ) ;
#7178 = AXIS2_PLACEMENT_3D ( 'NONE', #1732, #16253, #5605 ) ;
#7180 = SHAPE_DEFINITION_REPRESENTATION ( #10697, #13400 ) ;
#7181 = AXIS2_PLACEMENT_3D ( 'NONE', #12815, #21838, #5795 ) ;
#7182 = DIRECTION ( 'NONE',  ( 0.8660254037816071948, 0.5000000000049040771, 0.000000000000000000 ) ) ;
#7183 = DIRECTION ( 'NONE',  ( 0.000000000000000000, 1.000000000000000000, 0.000000000000000000 ) ) ;
#7184 = ORIENTED_EDGE ( 'NONE', *, *, #7931, .F. ) ;
#7185 = CARTESIAN_POINT ( 'NONE',  ( 18.19932492755376785, -3581.050454778146559, 2245.576347937810169 ) ) ;
#7186 = CARTESIAN_POINT ( 'NONE',  ( 137.8886907543135294, -3657.311334042124145, 2247.705354153496955 ) ) ;
#7187 = ORIENTED_EDGE ( 'NONE', *, *, #11514, .T. ) ;
#7188 = ORIENTED_EDGE ( 'NONE', *, *, #17653, .T. ) ;
#7189 = DIRECTION ( 'NONE',  ( 0.000000000000000000, 1.000000000000000000, 0.000000000000000000 ) ) ;
#7190 = ORIENTED_EDGE ( 'NONE', *, *, #13086, .T. ) ;
#7191 = ORIENTED_EDGE ( 'NONE', *, *, #7433, .F. ) ;
#7192 = ORIENTED_EDGE ( 'NONE', *, *, #7928, .T. ) ;
#7193 = CIRCLE ( 'NONE', #8310, 11.11250000000000071 ) ;
#7194 = AXIS2_PLACEMENT_3D ( 'NONE', #9726, #6226, #15011 ) ;
#7195 = DIRECTION ( 'NONE',  ( -0.8068916933244314471, 0.5906994119211830263, 0.000000000000000000 ) ) ;
#7196 = VERTEX_POINT ( 'NONE', #5121 ) ;
#7197 = VERTEX_POINT ( 'NONE', #16124 ) ;
#7198 = FACE_OUTER_BOUND ( 'NONE', #16069, .T. ) ;
#7199 = SECURITY_CLASSIFICATION_LEVEL ( 'unclassified' ) ;
#7200 = LINE ( 'NONE', #3785, #9167 ) ;
#7201 = LINE ( 'NONE', #14354, #5200 ) ;
#7202 = ORIENTED_EDGE ( 'NONE', *, *, #4376, .F. ) ;
#7203 = DIRECTION ( 'NONE',  ( 1.000000000000000000, 0.000000000000000000, 0.000000000000000000 ) ) ;
#7204 = FACE_BOUND ( 'NONE', #10927, .T. ) ;
#7205 = LINE ( 'NONE', #9425, #12085 ) ;
#7206 = FACE_OUTER_BOUND ( 'NONE', #11626, .T. ) ;
#7207 = VECTOR ( 'NONE', #5342, 1000.000000000000000 ) ;
#7208 = PERSON_AND_ORGANIZATION ( #5446, #1895 ) ;
#7209 = ORIENTED_EDGE ( 'NONE', *, *, #20562, .T. ) ;
#7210 = CARTESIAN_POINT ( 'NONE',  ( 0.000000000000000000, -3544.570000000000164, 2240.279999999999745 ) ) ;
#7211 = VERTEX_POINT ( 'NONE', #72 ) ;
#7212 = VECTOR ( 'NONE', #9810, 1000.000000000000000 ) ;
#7213 = B_SPLINE_CURVE_WITH_KNOTS ( 'NONE', 3,
 ( #4206, #5869, #18497, #5632, #350, #462, #7491, #14651, #12885, #22013, #14884, #14990, #2456, #9707, #9483, #3979, #7842 ),
 .UNSPECIFIED., .F., .F.,
 ( 4, 1, 1, 1, 1, 1, 1, 1, 1, 1, 1, 1, 1, 1, 4 ),
 ( 0.000000000000000000, 0.07142857142856999519, 0.1428571428570999946, 0.2142857142857000075, 0.2857142857143000203, 0.3571428571429000054, 0.4285714285713999594, 0.5000000000000000000, 0.5714285714286000406, 0.6428571428570999391, 0.7142857142856999797, 0.7857142857142999093, 0.8571428571429000609, 0.9285714285714000704, 0.9999948892528710553 ),
 .UNSPECIFIED. ) ;
#7214 = AXIS2_PLACEMENT_3D ( 'NONE', #19317, #22703, #10519 ) ;
#7215 = APPLIED_PERSON_AND_ORGANIZATION_ASSIGNMENT ( #3568, #12712, ( #12017 ) ) ;
#7216 = DIRECTION ( 'NONE',  ( -0.8928571428573600643, 0.4503400076038009403, 0.000000000000000000 ) ) ;
#7217 = CARTESIAN_POINT ( 'NONE',  ( 1.270000000000000018, -3544.570000000000164, 2240.279999999999745 ) ) ;
#7218 = ORIENTED_EDGE ( 'NONE', *, *, #14971, .T. ) ;
#7219 = DIRECTION ( 'NONE',  ( 0.000000000000000000, 1.000000000000000000, 0.000000000000000000 ) ) ;
#7220 = EDGE_CURVE ( 'NONE', #12269, #4791, #16950, .T. ) ;
#7221 = EDGE_CURVE ( 'NONE', #5432, #22780, #9323, .T. ) ;
#7222 = DIRECTION ( 'NONE',  ( 0.000000000000000000, 1.000000000000000000, 0.000000000000000000 ) ) ;
#7223 = CARTESIAN_POINT ( 'NONE',  ( 15.18950216440284784, -3580.932314744898576, 2239.010000000038417 ) ) ;
#7224 = DIRECTION ( 'NONE',  ( 0.000000000000000000, 0.000000000000000000, 1.000000000000000000 ) ) ;
#7225 = TOROIDAL_SURFACE ( 'NONE', #3091, 3.606799999999999784, 0.7620000000000000107 ) ;
#7226 = CYLINDRICAL_SURFACE ( 'NONE', #19263, 2.844800000000091700 ) ;
#7227 = ADVANCED_FACE ( 'NONE', ( #1588, #5233, #8749, #7108, #1709 ), #15895, .T. ) ;
#7228 = CARTESIAN_POINT ( 'NONE',  ( 139.6999999999999886, -3659.504999999999654, 2272.030000000000200 ) ) ;
#7229 = VERTEX_POINT ( 'NONE', #17759 ) ;
#7230 = VECTOR ( 'NONE', #8152, 1000.000000000000114 ) ;
#7231 = VECTOR ( 'NONE', #15494, 1000.000000000000000 ) ;
#7232 = APPLICATION_CONTEXT ( 'configuration controlled 3d designs of mechanical parts and assemblies' ) ;
#7233 = CARTESIAN_POINT ( 'NONE',  ( 95.25000000000000000, -3568.700000000000273, 2247.392000000000280 ) ) ;
#7234 = CARTESIAN_POINT ( 'NONE',  ( 12.70000000002683471, -3576.620370510378052, 2239.010000000078435 ) ) ;
#7235 = EDGE_CURVE ( 'NONE', #16346, #12999, #12613, .T. ) ;
#7236 = CARTESIAN_POINT ( 'NONE',  ( 136.9962509646508408, -3695.367664692730159, 2255.363857416606152 ) ) ;
#7237 = CARTESIAN_POINT ( 'NONE',  ( 7.657922162452776682, -3576.804516390709068, 2245.425293001298087 ) ) ;
#7238 = ORIENTED_EDGE ( 'NONE', *, *, #10577, .T. ) ;
#7239 = DIRECTION ( 'NONE',  ( 1.000000000000000000, 0.000000000000000000, 0.000000000000000000 ) ) ;
#7240 = EDGE_CURVE ( 'NONE', #4452, #15095, #8102, .T. ) ;
#7241 = CARTESIAN_POINT ( 'NONE',  ( 10.00638266403440824, -3543.659322602310112, 2255.389245125443722 ) ) ;
#7243 = VECTOR ( 'NONE', #18047, 999.9999999999998863 ) ;
#7242 = DATE_AND_TIME ( #92, #22840 ) ;
#7244 = EDGE_CURVE ( 'NONE', #14593, #21665, #1825, .T. ) ;
#7245 = DIRECTION ( 'NONE',  ( 0.000000000000000000, -1.000000000000000000, 0.000000000000000000 ) ) ;
#7246 = DIRECTION ( 'NONE',  ( -1.000000000000000000, 0.000000000000000000, 0.000000000000000000 ) ) ;
#7247 = CARTESIAN_POINT ( 'NONE',  ( 18.01287425285000410, -3657.399152860999493, 2246.630000000000109 ) ) ;
#7248 = TOROIDAL_SURFACE ( 'NONE', #21460, 3.606799999998999695, 0.7620000000000000107 ) ;
#7249 = CARTESIAN_POINT ( 'NONE',  ( 139.7000000001000046, -3576.802599999999984, 2242.820000000000164 ) ) ;
#7250 = AXIS2_PLACEMENT_3D ( 'NONE', #21115, #3294, #17232 ) ;
#7251 = ORIENTED_EDGE ( 'NONE', *, *, #9705, .F. ) ;
#7252 = DIRECTION ( 'NONE',  ( 1.000000000000000000, 0.000000000000000000, 0.000000000000000000 ) ) ;
#7253 = EDGE_LOOP ( 'NONE', ( #13675, #19005, #9205, #21534 ) ) ;
#7254 = DIRECTION ( 'NONE',  ( 0.000000000000000000, -1.000000000000000000, 4.457650181899999573E-12 ) ) ;
#7255 = ADVANCED_FACE ( 'NONE', ( #6725 ), #15960, .T. ) ;
#7256 = PLANE ( 'NONE',  #7339 ) ;
#7257 = ORIENTED_EDGE ( 'NONE', *, *, #19810, .T. ) ;
#7258 = AXIS2_PLACEMENT_3D ( 'NONE', #4625, #19160, #2983 ) ;
#7259 = VERTEX_POINT ( 'NONE', #17359 ) ;
#7260 = CARTESIAN_POINT ( 'NONE',  ( 127.0000000000000000, -3670.300000000000182, 2259.837999999999738 ) ) ;
#7261 = DIRECTION ( 'NONE',  ( 1.000000000000000000, 0.000000000000000000, 0.000000000000000000 ) ) ;
#7262 = ORIENTED_EDGE ( 'NONE', *, *, #9679, .F. ) ;
#7263 = CARTESIAN_POINT ( 'NONE',  ( 137.7193482430640188, -3581.537511303820338, 2248.354490200028522 ) ) ;
#7264 = ORIENTED_EDGE ( 'NONE', *, *, #12299, .F. ) ;
#7265 = CARTESIAN_POINT ( 'NONE',  ( 57.14999999999999858, -3568.700000000000273, 2247.392000000000280 ) ) ;
#7266 = DATE_AND_TIME ( #3737, #16118 ) ;
#7267 = FACE_OUTER_BOUND ( 'NONE', #16763, .T. ) ;
#7268 = CARTESIAN_POINT ( 'NONE',  ( -8.890000000022000748, -3661.486200000000281, 2245.060313203000078 ) ) ;
#7269 = AXIS2_PLACEMENT_3D ( 'NONE', #5732, #7705, #9352 ) ;
#7270 = CARTESIAN_POINT ( 'NONE',  ( 0.000000000000000000, -3544.061999999999898, 2295.829799999999977 ) ) ;
#7271 = CARTESIAN_POINT ( 'NONE',  ( -6.349999999999999645, -3584.320999999999913, 2247.392000000000280 ) ) ;
#7272 = CIRCLE ( 'NONE', #15890, 1.904999999999823501 ) ;
#7273 = CARTESIAN_POINT ( 'NONE',  ( 141.8684782314425661, -3577.653504331623481, 2249.968348377236453 ) ) ;
#7274 = ORIENTED_EDGE ( 'NONE', *, *, #11726, .F. ) ;
#7275 = CARTESIAN_POINT ( 'NONE',  ( 134.4883907600942052, -3577.149724370994591, 2245.118708806262930 ) ) ;
#7276 = LINE ( 'NONE', #14200, #927 ) ;
#7277 = VERTEX_POINT ( 'NONE', #19137 ) ;
#7278 = DIRECTION ( 'NONE',  ( 0.9296367896517967466, -0.3684771896955098547, 0.000000000000000000 ) ) ;
#7279 = CARTESIAN_POINT ( 'NONE',  ( 7.238999999999998991, -3639.502500000000055, 2290.622800000000552 ) ) ;
#7280 = EDGE_CURVE ( 'NONE', #13787, #22588, #21203, .T. ) ;
#7281 = ADVANCED_FACE ( 'NONE', ( #6841 ), #5074, .T. ) ;
#7282 = ORIENTED_EDGE ( 'NONE', *, *, #14046, .F. ) ;
#7283 = EDGE_CURVE ( 'NONE', #22625, #15231, #912, .T. ) ;
#7284 = CARTESIAN_POINT ( 'NONE',  ( 151.4000000000000057, -3544.061999999999898, 2296.591799999999694 ) ) ;
#7285 = DIRECTION ( 'NONE',  ( -2.324635735433000053E-14, 2.336881798971000105E-14, -1.000000000000000000 ) ) ;
#7286 = AXIS2_PLACEMENT_3D ( 'NONE', #13666, #1587, #10261 ) ;
#7287 = ORIENTED_EDGE ( 'NONE', *, *, #12957, .T. ) ;
#7288 = TOROIDAL_SURFACE ( 'NONE', #5046, 3.606799999999999784, 0.7620000000000000107 ) ;
#7289 = DIRECTION ( 'NONE',  ( -1.000000000000000000, 1.224646799147353207E-16, 0.000000000000000000 ) ) ;
#7290 = DIRECTION ( 'NONE',  ( 0.000000000000000000, 0.000000000000000000, -1.000000000000000000 ) ) ;
#7291 =( NAMED_UNIT ( * ) SI_UNIT ( $, .STERADIAN. ) SOLID_ANGLE_UNIT ( ) );
#7292 = AXIS2_PLACEMENT_3D ( 'NONE', #2408, #19152, #19036 ) ;
#7293 = DIRECTION ( 'NONE',  ( 0.000000000000000000, 0.000000000000000000, -1.000000000000000000 ) ) ;
#7294 = EDGE_CURVE ( 'NONE', #6851, #13920, #8855, .T. ) ;
#7295 = LINE ( 'NONE', #11157, #18238 ) ;
#7296 = COORDINATED_UNIVERSAL_TIME_OFFSET ( 0, 0, .AHEAD. ) ;
#7297 = CYLINDRICAL_SURFACE ( 'NONE', #1019, 6.349999999999855760 ) ;
#7298 = CARTESIAN_POINT ( 'NONE',  ( 9.998047855982495236, -3695.360820975178285, 2255.368362556688680 ) ) ;
#7299 = EDGE_LOOP ( 'NONE', ( #15669, #1580, #5187, #19780 ) ) ;
#7300 = DIRECTION ( 'NONE',  ( 0.000000000000000000, 0.000000000000000000, 1.000000000000000000 ) ) ;
#7301 = EDGE_CURVE ( 'NONE', #18199, #20633, #22634, .T. ) ;
#7302 = DIRECTION ( 'NONE',  ( -1.000000000000000000, 0.000000000000000000, 0.000000000000000000 ) ) ;
#7303 = EDGE_CURVE ( 'NONE', #22029, #9475, #2479, .T. ) ;
#7304 = ORIENTED_EDGE ( 'NONE', *, *, #17687, .T. ) ;
#7305 = TOROIDAL_SURFACE ( 'NONE', #8423, 3.606799999999999784, 0.7620000000000000107 ) ;
#7306 = CARTESIAN_POINT ( 'NONE',  ( 138.1068462689100613, -3661.863663675439511, 2249.656022096149172 ) ) ;
#7307 = AXIS2_PLACEMENT_3D ( 'NONE', #2572, #6566, #17205 ) ;
#7308 = EDGE_LOOP ( 'NONE', ( #10163, #21900 ) ) ;
#7309 = AXIS2_PLACEMENT_3D ( 'NONE', #5415, #22571, #4650 ) ;
#7310 = ORIENTED_EDGE ( 'NONE', *, *, #14118, .F. ) ;
#7311 = ORIENTED_EDGE ( 'NONE', *, *, #17903, .T. ) ;
#7312 = DIRECTION ( 'NONE',  ( 1.000000000000000000, 0.000000000000000000, -1.224646799147353207E-16 ) ) ;
#7313 = VERTEX_POINT ( 'NONE', #4952 ) ;
#7314 = EDGE_LOOP ( 'NONE', ( #17990, #11604 ) ) ;
#7315 = CARTESIAN_POINT ( 'NONE',  ( -12.31900000000012696, -3665.601000000000113, 2247.392000000000280 ) ) ;
#7316 = APPROVAL_ROLE ( '' ) ;
#7317 = CARTESIAN_POINT ( 'NONE',  ( 38.10000000000000142, -3594.099999999999909, 2239.771999999999935 ) ) ;
#7318 = CARTESIAN_POINT ( 'NONE',  ( 9.855200000000680305, -3659.956214629480201, 2256.063559999999597 ) ) ;
#7319 = ORIENTED_EDGE ( 'NONE', *, *, #351, .T. ) ;
#7320 = DIRECTION ( 'NONE',  ( -1.000000000000000000, 0.000000000000000000, 0.000000000000000000 ) ) ;
#7321 = FACE_OUTER_BOUND ( 'NONE', #15142, .T. ) ;
#7322 = LINE ( 'NONE', #11058, #7603 ) ;
#7323 = TOROIDAL_SURFACE ( 'NONE', #16658, 4.114799999999999791, 1.270000000000000018 ) ;
#7324 = TOROIDAL_SURFACE ( 'NONE', #5827, 3.606799999999999784, 0.7620000000000000107 ) ;
#7325 = DIRECTION ( 'NONE',  ( -2.903809793931999834E-13, 4.457650181899999573E-12, 1.000000000000000000 ) ) ;
#7326 = PERSON_AND_ORGANIZATION_ROLE ( 'classification_officer' ) ;
#7327 = CIRCLE ( 'NONE', #10306, 3.606800000000000228 ) ;
#7328 = ORIENTED_EDGE ( 'NONE', *, *, #12505, .T. ) ;
#7329 = AXIS2_PLACEMENT_3D ( 'NONE', #10530, #22821, #1615 ) ;
#7330 = FACE_OUTER_BOUND ( 'NONE', #17216, .T. ) ;
#7331 = ORIENTED_EDGE ( 'NONE', *, *, #12597, .T. ) ;
#7332 = DIRECTION ( 'NONE',  ( 0.000000000000000000, 0.000000000000000000, 1.000000000000000000 ) ) ;
#7333 = DIRECTION ( 'NONE',  ( 0.000000000000000000, 0.000000000000000000, -1.000000000000000000 ) ) ;
#7334 = ORIENTED_EDGE ( 'NONE', *, *, #3052, .F. ) ;
#7335 = DIRECTION ( 'NONE',  ( -1.000000000000000000, 0.000000000000000000, 0.000000000000000000 ) ) ;
#7336 = CIRCLE ( 'NONE', #234, 0.7619999999999987894 ) ;
#7337 = LINE ( 'NONE', #5348, #1298 ) ;
#7338 = CARTESIAN_POINT ( 'NONE',  ( 64.76999999999999602, -3568.700000000000273, 2289.213099999999940 ) ) ;
#7339 = AXIS2_PLACEMENT_3D ( 'NONE', #106, #12988, #5738 ) ;
#7340 = CARTESIAN_POINT ( 'NONE',  ( 95.25000000000000000, -3568.700000000000273, 2247.392000000000280 ) ) ;
#7341 = AXIS2_PLACEMENT_3D ( 'NONE', #3325, #20793, #1688 ) ;
#7342 = CARTESIAN_POINT ( 'NONE',  ( 18.12143270522780014, -3657.696842364385247, 2245.934643265300110 ) ) ;
#7343 = ORIENTED_EDGE ( 'NONE', *, *, #2258, .F. ) ;
#7344 = CARTESIAN_POINT ( 'NONE',  ( 147.5630070217191587, -3695.514947978554574, 2259.991585417506030 ) ) ;
#7345 = LINE ( 'NONE', #21524, #8022 ) ;
#7346 = AXIS2_PLACEMENT_3D ( 'NONE', #306, #5929, #7557 ) ;
#7347 = DIRECTION ( 'NONE',  ( 0.000000000000000000, 1.000000000000000000, 0.000000000000000000 ) ) ;
#7348 = APPROVAL ( #12884, 'UNSPECIFIED' ) ;
#7349 = CARTESIAN_POINT ( 'NONE',  ( 104.4447999999999865, -3568.700000000000273, 2261.869999999999891 ) ) ;
#7350 = DIRECTION ( 'NONE',  ( -1.000000000000000000, 0.000000000000000000, 0.000000000000000000 ) ) ;
#7351 = CARTESIAN_POINT ( 'NONE',  ( 137.1440299052392788, -3694.748620250294152, 2255.734053407186821 ) ) ;
#7352 = VERTEX_POINT ( 'NONE', #1077 ) ;
#7353 = CARTESIAN_POINT ( 'NONE',  ( 7.099392720542782698, -3578.355474235146630, 2244.591332851781317 ) ) ;
#7354 = EDGE_LOOP ( 'NONE', ( #10703, #16971, #17607, #13518 ) ) ;
#7355 = PERSON_AND_ORGANIZATION ( #5446, #1895 ) ;
#7356 = ADVANCED_FACE ( 'NONE', ( #11872 ), #2960, .T. ) ;
#7357 = FACE_OUTER_BOUND ( 'NONE', #13844, .T. ) ;
#7358 = AXIS2_PLACEMENT_3D ( 'NONE', #4284, #18576, #7914 ) ;
#7359 = DIRECTION ( 'NONE',  ( 0.000000000000000000, 0.000000000000000000, 1.000000000000000000 ) ) ;
#7360 = COORDINATED_UNIVERSAL_TIME_OFFSET ( 0, 0, .AHEAD. ) ;
#7361 = EDGE_CURVE ( 'NONE', #1371, #10059, #10104, .T. ) ;
#7362 = CARTESIAN_POINT ( 'NONE',  ( 8.088613972650000150, -3576.119152860999748, 2246.630000000000109 ) ) ;
#7363 = CIRCLE ( 'NONE', #15967, 2.844800000000001550 ) ;
#7364 = FACE_OUTER_BOUND ( 'NONE', #15481, .T. ) ;
#7365 = CIRCLE ( 'NONE', #7747, 0.7619999999999294005 ) ;
#7366 = CARTESIAN_POINT ( 'NONE',  ( 104.4447999999999865, -3619.500000000000000, 2261.869999999999891 ) ) ;
#7367 = ORIENTED_EDGE ( 'NONE', *, *, #13534, .F. ) ;
#7368 = CYLINDRICAL_SURFACE ( 'NONE', #15865, 0.7619999999999294005 ) ;
#7369 = ORIENTED_EDGE ( 'NONE', *, *, #20058, .T. ) ;
#7370 = CARTESIAN_POINT ( 'NONE',  ( 17.31138602737999932, -3662.880847139000252, 2246.630000000000109 ) ) ;
#7371 = CARTESIAN_POINT ( 'NONE',  ( 12.69999999999999929, -3639.502500000000055, 2263.571799999999712 ) ) ;
#7372 = ORIENTED_EDGE ( 'NONE', *, *, #1329, .T. ) ;
#7373 = DIRECTION ( 'NONE',  ( -1.000000000000000000, 0.000000000000000000, 0.000000000000000000 ) ) ;
#7374 = TOROIDAL_SURFACE ( 'NONE', #22321, 3.606799999998999695, 0.7620000000000000107 ) ;
#7375 = EDGE_LOOP ( 'NONE', ( #5317, #16502, #22269, #3085 ) ) ;
#7376 = CARTESIAN_POINT ( 'NONE',  ( 142.3712313342016671, -3695.282573427255556, 2255.445352725234443 ) ) ;
#7377 = CARTESIAN_POINT ( 'NONE',  ( 50.79999999999999716, -3568.700000000000273, 2239.009999999999764 ) ) ;
#7378 = EDGE_LOOP ( 'NONE', ( #3825, #9875, #9330, #6334, #1208, #12467, #6913, #6546, #240, #41 ) ) ;
#7379 = EDGE_CURVE ( 'NONE', #18081, #19890, #13625, .T. ) ;
#7380 = CARTESIAN_POINT ( 'NONE',  ( 137.0759654552891220, -3580.596807917107526, 2249.647026203515452 ) ) ;
#7381 = ORIENTED_EDGE ( 'NONE', *, *, #5841, .T. ) ;
#7382 = FACE_OUTER_BOUND ( 'NONE', #17505, .T. ) ;
#7383 = EDGE_CURVE ( 'NONE', #5536, #5355, #16686, .T. ) ;
#7384 = APPROVAL_ROLE ( '' ) ;
#7385 = EDGE_CURVE ( 'NONE', #10237, #3900, #15575, .T. ) ;
#7386 = LINE ( 'NONE', #15825, #3726 ) ;
#7387 = LINE ( 'NONE', #7268, #3628 ) ;
#7388 =( BOUNDED_CURVE ( )  B_SPLINE_CURVE ( 3, ( #9740, #2822, #2493, #13610 ),
 .UNSPECIFIED., .F., .F. ) 
 B_SPLINE_CURVE_WITH_KNOTS ( ( 4, 4 ),
 ( -8.881784197001252323E-16, 1.570796326722519565 ),
 .UNSPECIFIED. ) 
 CURVE ( )  GEOMETRIC_REPRESENTATION_ITEM ( )  RATIONAL_B_SPLINE_CURVE ( ( 1.000000000000000000, 0.8047378541414241804, 0.8047378541414241804, 1.000000000000000000 ) ) 
 REPRESENTATION_ITEM ( '' )  );
#7389 = CARTESIAN_POINT ( 'NONE',  ( 15.18950216452952162, -3578.057685255022534, 2239.009999999890624 ) ) ;
#7390 = DIRECTION ( 'NONE',  ( -1.000000000000000000, 5.461016542361937364E-28, 2.336881798970999789E-14 ) ) ;
#7391 = AXIS2_PLACEMENT_3D ( 'NONE', #17806, #1870, #14300 ) ;
#7392 = CARTESIAN_POINT ( 'NONE',  ( 139.0044331210974349, -3576.736148240796410, 2249.284738289012694 ) ) ;
#7393 = PERSON ( 'NAUO-PER3', 'UNSPECIFIED', 'UNSPECIFIED', ('UNSPECIFIED'), ('UNSPECIFIED'), ('UNSPECIFIED') ) ;
#7394 = VERTEX_POINT ( 'NONE', #13754 ) ;
#7395 = CARTESIAN_POINT ( 'NONE',  ( 134.8618250315517457, -3576.452994732182106, 2245.875428656681379 ) ) ;
#7396 = VECTOR ( 'NONE', #15079, 1000.000000000000000 ) ;
#7397 = AXIS2_PLACEMENT_3D ( 'NONE', #12072, #20747, #22492 ) ;
#7398 = DIRECTION ( 'NONE',  ( 1.000000000000000000, 0.000000000000000000, 0.000000000000000000 ) ) ;
#7399 = ORIENTED_EDGE ( 'NONE', *, *, #10943, .T. ) ;
#7400 = DIRECTION ( 'NONE',  ( 4.316835273014999614E-14, 1.000000000000000000, 2.309184719176999840E-12 ) ) ;
#7401 = PLANE ( 'NONE',  #1612 ) ;
#7402 = ORIENTED_EDGE ( 'NONE', *, *, #20299, .T. ) ;
#7403 = DIRECTION ( 'NONE',  ( 0.000000000000000000, 0.000000000000000000, -1.000000000000000000 ) ) ;
#7404 = CARTESIAN_POINT ( 'NONE',  ( 47.95519999999999783, -3568.700000000000273, 2259.837999999999738 ) ) ;
#7405 = VERTEX_POINT ( 'NONE', #8589 ) ;
#7406 = CIRCLE ( 'NONE', #4041, 5.080000000000000959 ) ;
#7407 = DIRECTION ( 'NONE',  ( 1.000000000000000000, 0.000000000000000000, 3.996303350731721563E-14 ) ) ;
#7408 = DIRECTION ( 'NONE',  ( 0.6887494619135663410, 0.000000000000000000, -0.7249994335954840219 ) ) ;
#7409 =( LENGTH_UNIT ( ) NAMED_UNIT ( * ) SI_UNIT ( .MILLI., .METRE. ) );
#7410 = CARTESIAN_POINT ( 'NONE',  ( -12.69999999999999929, -3578.860000000000127, 2247.392000000000280 ) ) ;
#7411 = CARTESIAN_POINT ( 'NONE',  ( 12.69999999999999929, -3659.504999999999654, 2244.978999999999814 ) ) ;
#7412 = PRODUCT_CONTEXT ( 'NONE', #2877, 'mechanical' ) ;
#7413 = CIRCLE ( 'NONE', #11159, 0.7619999999999294005 ) ;
#7414 = EDGE_CURVE ( 'NONE', #15102, #22318, #10457, .T. ) ;
#7415 = CARTESIAN_POINT ( 'NONE',  ( 20.52663054042999846, -3694.556024844999683, 2260.595783923999988 ) ) ;
#7416 = CYLINDRICAL_SURFACE ( 'NONE', #15054, 1.269999999999882334 ) ;
#7417 = ORIENTED_EDGE ( 'NONE', *, *, #17236, .T. ) ;
#7418 = DIRECTION ( 'NONE',  ( 0.000000000000000000, 0.000000000000000000, -1.000000000000000000 ) ) ;
#7419 = ADVANCED_FACE ( 'NONE', ( #6375 ), #11985, .T. ) ;
#7420 = CARTESIAN_POINT ( 'NONE',  ( 137.8759894827288690, -3657.321687586756980, 2247.788848385796882 ) ) ;
#7421 = EDGE_CURVE ( 'NONE', #11162, #19328, #11742, .T. ) ;
#7422 = ORIENTED_EDGE ( 'NONE', *, *, #3359, .F. ) ;
#7423 = CARTESIAN_POINT ( 'NONE',  ( 137.8845111942463859, -3661.695361931427669, 2249.774021930013532 ) ) ;
#7424 = VECTOR ( 'NONE', #15253, 1000.000000000000000 ) ;
#7425 = VERTEX_POINT ( 'NONE', #4722 ) ;
#7426 = EDGE_CURVE ( 'NONE', #9059, #16839, #8361, .T. ) ;
#7427 = ORIENTED_EDGE ( 'NONE', *, *, #22581, .F. ) ;
#7428 = DIRECTION ( 'NONE',  ( 0.000000000000000000, 0.000000000000000000, -1.000000000000000000 ) ) ;
#7429 = ORIENTED_EDGE ( 'NONE', *, *, #16235, .F. ) ;
#7430 = ORIENTED_EDGE ( 'NONE', *, *, #4635, .T. ) ;
#7431 = CARTESIAN_POINT ( 'NONE',  ( -8.890000000008999592, -3662.832400000000234, 2247.392000000000280 ) ) ;
#7432 = CARTESIAN_POINT ( 'NONE',  ( 22.54063073453000143, -3694.938000000000102, 2275.001800000000003 ) ) ;
#7433 = EDGE_CURVE ( 'NONE', #1958, #3991, #15495, .T. ) ;
#7434 = ORIENTED_EDGE ( 'NONE', *, *, #4547, .F. ) ;
#7435 = DIRECTION ( 'NONE',  ( 0.000000000000000000, 1.000000000000000000, 0.000000000000000000 ) ) ;
#7436 = EDGE_CURVE ( 'NONE', #16534, #22243, #10729, .T. ) ;
#7437 = CARTESIAN_POINT ( 'NONE',  ( 25.39999999999999858, -3660.140000000000327, 2244.547199999999975 ) ) ;
#7438 = VECTOR ( 'NONE', #12936, 1000.000000000000000 ) ;
#7439 = FACE_OUTER_BOUND ( 'NONE', #19422, .T. ) ;
#7440 = SECURITY_CLASSIFICATION_LEVEL ( 'unclassified' ) ;
#7441 = CARTESIAN_POINT ( 'NONE',  ( 131.8826930129156096, -3543.564485452164263, 2260.105821329443188 ) ) ;
#7442 = ORIENTED_EDGE ( 'NONE', *, *, #9152, .T. ) ;
#7443 = CIRCLE ( 'NONE', #1063, 2.873832635400752622 ) ;
#7444 = DIRECTION ( 'NONE',  ( 0.000000000000000000, 0.5000000000031962211, -0.8660254037825932949 ) ) ;
#7445 = EDGE_CURVE ( 'NONE', #11629, #12173, #4825, .T. ) ;
#7446 = CARTESIAN_POINT ( 'NONE',  ( 8.062487613724396596, -3662.845158696698491, 2246.501631804077533 ) ) ;
#7447 = DIRECTION ( 'NONE',  ( 1.000000000000000000, 0.000000000000000000, 0.000000000000000000 ) ) ;
#7448 = ORIENTED_EDGE ( 'NONE', *, *, #12807, .F. ) ;
#7449 = PLANE ( 'NONE',  #260 ) ;
#7450 = CARTESIAN_POINT ( 'NONE',  ( 18.16100000000000136, -3599.497499999999945, 2290.622800000000097 ) ) ;
#7451 = DIRECTION ( 'NONE',  ( 0.000000000000000000, 0.000000000000000000, 1.000000000000000000 ) ) ;
#7452 = DIRECTION ( 'NONE',  ( 0.000000000000000000, 0.000000000000000000, -1.000000000000000000 ) ) ;
#7453 = DIRECTION ( 'NONE',  ( 0.000000000000000000, 0.000000000000000000, -1.000000000000000000 ) ) ;
#7454 = ORIENTED_EDGE ( 'NONE', *, *, #10999, .F. ) ;
#7455 = CARTESIAN_POINT ( 'NONE',  ( 38.10000000000000142, -3594.099999999999909, 2239.009999999999764 ) ) ;
#7456 = LINE ( 'NONE', #18342, #21873 ) ;
#7457 = AXIS2_PLACEMENT_3D ( 'NONE', #13529, #22889, #17037 ) ;
#7458 = LINE ( 'NONE', #2190, #9568 ) ;
#7459 = ADVANCED_FACE ( 'NONE', ( #10098 ), #12330, .T. ) ;
#7460 = DIRECTION ( 'NONE',  ( 0.000000000000000000, 0.000000000000000000, -1.000000000000000000 ) ) ;
#7461 = CARTESIAN_POINT ( 'NONE',  ( 142.4686189914979764, -3543.507962130772285, 2255.201647170270917 ) ) ;
#7462 = DIRECTION ( 'NONE',  ( -1.000000000000000000, 0.000000000000000000, 0.000000000000000000 ) ) ;
#7463 = CARTESIAN_POINT ( 'NONE',  ( 10.36831320283000046, -3600.843699999999899, 2292.781800000000203 ) ) ;
#7464 = ORIENTED_EDGE ( 'NONE', *, *, #12866, .T. ) ;
#7465 = COORDINATED_UNIVERSAL_TIME_OFFSET ( 0, 0, .AHEAD. ) ;
#7466 = DIRECTION ( 'NONE',  ( 0.000000000000000000, 0.000000000000000000, 1.000000000000000000 ) ) ;
#7467 = LINE ( 'NONE', #12394, #21996 ) ;
#7468 = CALENDAR_DATE ( 2026, 26, 10 ) ;
#7469 = CARTESIAN_POINT ( 'NONE',  ( 139.6999999999999886, -3582.627340905000437, 2239.009999999999764 ) ) ;
#7470 = CARTESIAN_POINT ( 'NONE',  ( 38.10000000000000142, -3644.899999999999636, 2261.869999999999891 ) ) ;
#7471 = AXIS2_PLACEMENT_3D ( 'NONE', #7892, #16671, #4034 ) ;
#7472 = ORIENTED_EDGE ( 'NONE', *, *, #19751, .T. ) ;
#7473 = DIRECTION ( 'NONE',  ( 1.000000000000000000, 0.000000000000000000, 0.000000000000000000 ) ) ;
#7474 = ORIENTED_EDGE ( 'NONE', *, *, #6379, .T. ) ;
#7475 = CARTESIAN_POINT ( 'NONE',  ( 12.69999999999999929, -3599.497499999999945, 2288.971800000000258 ) ) ;
#7476 = VERTEX_POINT ( 'NONE', #1543 ) ;
#7477 = FACE_OUTER_BOUND ( 'NONE', #22003, .T. ) ;
#7478 = LINE ( 'NONE', #13553, #5471 ) ;
#7479 = VERTEX_POINT ( 'NONE', #10335 ) ;
#7480 = CARTESIAN_POINT ( 'NONE',  ( 139.6999999999999886, -3659.504999999999654, 2270.760000000000218 ) ) ;
#7481 = AXIS2_PLACEMENT_3D ( 'NONE', #18967, #22464, #17311 ) ;
#7482 = ORIENTED_EDGE ( 'NONE', *, *, #19024, .T. ) ;
#7483 = CARTESIAN_POINT ( 'NONE',  ( 142.2400000001210572, -3694.509865590614027, 2255.773999999871648 ) ) ;
#7484 = CARTESIAN_POINT ( 'NONE',  ( 1.270000000000000018, -3578.860000000000127, 2247.392000000000280 ) ) ;
#7485 = PRODUCT_DEFINITION_FORMATION_WITH_SPECIFIED_SOURCE ( 'ANY', '', #15546, .NOT_KNOWN. ) ;
#7486 = ORIENTED_EDGE ( 'NONE', *, *, #15017, .F. ) ;
#7487 = CARTESIAN_POINT ( 'NONE',  ( 137.2263574705312976, -3580.899882066081773, 2249.375081330945704 ) ) ;
#7488 = ORIENTED_EDGE ( 'NONE', *, *, #8688, .T. ) ;
#7489 = CARTESIAN_POINT ( 'NONE',  ( 9.525000000091798924, -3694.938000000000102, 2281.351800000090861 ) ) ;
#7490 = CALENDAR_DATE ( 2026, 26, 10 ) ;
#7491 = CARTESIAN_POINT ( 'NONE',  ( 15.11851036462000053, -3641.011922182000035, 2279.551735152999754 ) ) ;
#7492 = DIRECTION ( 'NONE',  ( -1.000000000000000000, -1.165588477296775430E-12, 0.000000000000000000 ) ) ;
#7493 = AXIS2_PLACEMENT_3D ( 'NONE', #21074, #16033, #14042 ) ;
#7494 = DIRECTION ( 'NONE',  ( 0.000000000000000000, -1.000000000000000000, 0.000000000000000000 ) ) ;
#7495 = DIRECTION ( 'NONE',  ( -0.000000000000000000, -1.000000000000000000, -0.000000000000000000 ) ) ;
#7496 = LOCAL_TIME ( 17, 37, 43.00000000000000000, #4321 ) ;
#7497 = CARTESIAN_POINT ( 'NONE',  ( 138.4977950649703473, -3576.916347349343141, 2249.469419588345772 ) ) ;
#7498 = ORIENTED_EDGE ( 'NONE', *, *, #14013, .T. ) ;
#7499 = PRODUCT_DEFINITION_FORMATION_WITH_SPECIFIED_SOURCE ( 'ANY', '', #16320, .NOT_KNOWN. ) ;
#7500 = CARTESIAN_POINT ( 'NONE',  ( 12.69999999999999929, -3639.502500000000055, 2296.210799999999836 ) ) ;
#7501 = EDGE_CURVE ( 'NONE', #17371, #2232, #18928, .T. ) ;
#7502 = ORIENTED_EDGE ( 'NONE', *, *, #11710, .F. ) ;
#7503 = DIRECTION ( 'NONE',  ( -1.000000000000000000, 0.000000000000000000, 0.000000000000000000 ) ) ;
#7504 = ORIENTED_EDGE ( 'NONE', *, *, #20973, .F. ) ;
#7505 = EDGE_CURVE ( 'NONE', #11737, #7086, #17600, .T. ) ;
#7506 = CARTESIAN_POINT ( 'NONE',  ( 11.12257588577000078, -3581.868010977999802, 2257.704312134999782 ) ) ;
#7507 = CARTESIAN_POINT ( 'NONE',  ( 12.69999999999999929, -3659.504999999999654, 2270.760000000000218 ) ) ;
#7508 = EDGE_CURVE ( 'NONE', #15124, #11974, #3385, .T. ) ;
#7509 = EDGE_LOOP ( 'NONE', ( #16209, #5661, #16386, #10276 ) ) ;
#7510 = CARTESIAN_POINT ( 'NONE',  ( 15.49598722424000030, -3660.053501552999933, 2257.950090894999903 ) ) ;
#7511 = CARTESIAN_POINT ( 'NONE',  ( 20.32000000000000028, -3660.140000000000327, 2247.392000000000280 ) ) ;
#7512 = EDGE_LOOP ( 'NONE', ( #13808, #16868, #4512, #5296 ) ) ;
#7513 = CARTESIAN_POINT ( 'NONE',  ( 0.000000000000000000, -3694.430000000000291, 2259.329999999999927 ) ) ;
#7514 = DIRECTION ( 'NONE',  ( -0.5000000000047110094, -0.8660254037817188832, 0.000000000000000000 ) ) ;
#7515 = EDGE_CURVE ( 'NONE', #9827, #14706, #12680, .T. ) ;
#7516 = DIRECTION ( 'NONE',  ( 0.000000000000000000, 0.000000000000000000, -1.000000000000000000 ) ) ;
#7517 = CARTESIAN_POINT ( 'NONE',  ( 141.5301317845463132, -3581.673074589064527, 2246.966346727968357 ) ) ;
#7518 = VERTEX_POINT ( 'NONE', #1307 ) ;
#7519 = LOCAL_TIME ( 17, 37, 43.00000000000000000, #19862 ) ;
#7520 = CARTESIAN_POINT ( 'NONE',  ( 139.6999999997612747, -3662.637340905137989, 2239.009999999999764 ) ) ;
#7521 = DATE_AND_TIME ( #2587, #21708 ) ;
#7522 = CARTESIAN_POINT ( 'NONE',  ( 12.69999999999999929, -3637.597499999999854, 2263.571799999999712 ) ) ;
#7523 = CARTESIAN_POINT ( 'NONE',  ( 34.49320000000000164, -3644.899999999999636, 2239.009999999999764 ) ) ;
#7524 = EDGE_LOOP ( 'NONE', ( #9493, #5812, #15911, #12581, #13745, #1009, #14284, #16014 ) ) ;
#7525 = CARTESIAN_POINT ( 'NONE',  ( 18.26645764376696235, -3580.789478182200128, 2245.301509789812371 ) ) ;
#7526 = EDGE_CURVE ( 'NONE', #14294, #21382, #22828, .T. ) ;
#7527 = CARTESIAN_POINT ( 'NONE',  ( 136.8709027835478196, -3659.159706171275047, 2250.069058248565852 ) ) ;
#7528 = AXIS2_PLACEMENT_3D ( 'NONE', #10121, #15290, #7912 ) ;
#7529 = ORIENTED_EDGE ( 'NONE', *, *, #5391, .T. ) ;
#7530 = ORIENTED_EDGE ( 'NONE', *, *, #8131, .F. ) ;
#7531 = CARTESIAN_POINT ( 'NONE',  ( 141.2546625656592028, -3661.887891249280983, 2249.636713181481355 ) ) ;
#7532 = EDGE_LOOP ( 'NONE', ( #19207, #13120, #8666, #13637 ) ) ;
#7533 = ORIENTED_EDGE ( 'NONE', *, *, #5800, .T. ) ;
#7534 = ADVANCED_FACE ( 'NONE', ( #8473 ), #5069, .F. ) ;
#7535 = DIRECTION ( 'NONE',  ( -1.000000000000000000, 0.000000000000000000, 0.000000000000000000 ) ) ;
#7536 = VERTEX_POINT ( 'NONE', #8353 ) ;
#7537 = CARTESIAN_POINT ( 'NONE',  ( -8.890000000024000926, -3576.167599999999766, 2247.392000000000280 ) ) ;
#7538 = DATE_AND_TIME ( #9419, #6057 ) ;
#7539 = DIRECTION ( 'NONE',  ( 1.000000000000000000, 0.000000000000000000, 0.000000000000000000 ) ) ;
#7540 = CIRCLE ( 'NONE', #1545, 6.349999999999855760 ) ;
#7541 = EDGE_LOOP ( 'NONE', ( #6428, #8632, #4442, #3896, #18945, #6525, #9014, #21457 ) ) ;
#7542 = CIRCLE ( 'NONE', #15776, 5.714999999999999858 ) ;
#7543 = EDGE_CURVE ( 'NONE', #3230, #22365, #21006, .T. ) ;
#7544 = CARTESIAN_POINT ( 'NONE',  ( 7.619999999999999218, -3639.502500000000055, 2290.622800000000097 ) ) ;
#7545 = DIRECTION ( 'NONE',  ( 1.000000000000000000, 0.000000000000000000, 0.000000000000000000 ) ) ;
#7546 = CARTESIAN_POINT ( 'NONE',  ( 9.855200508370408841, -3579.494995334292526, 2257.962940200996854 ) ) ;
#7547 = DIRECTION ( 'NONE',  ( -1.000000000000000000, 0.000000000000000000, 0.000000000000000000 ) ) ;
#7548 = DATE_AND_TIME ( #7895, #7158 ) ;
#7549 = CARTESIAN_POINT ( 'NONE',  ( 56.10057940169000545, -3544.061999999999898, 2275.211350432000472 ) ) ;
#7550 = ORIENTED_EDGE ( 'NONE', *, *, #22002, .T. ) ;
#7551 = FACE_OUTER_BOUND ( 'NONE', #9609, .T. ) ;
#7552 = DIRECTION ( 'NONE',  ( 0.7071067811864976127, 0.000000000000000000, 0.7071067811865975328 ) ) ;
#7553 = DIRECTION ( 'NONE',  ( 0.000000000000000000, 0.000000000000000000, 1.000000000000000000 ) ) ;
#7554 = ORIENTED_EDGE ( 'NONE', *, *, #7515, .F. ) ;
#7555 = CIRCLE ( 'NONE', #4190, 0.7619999999999987894 ) ;
#7556 = EDGE_CURVE ( 'NONE', #19621, #7999, #1507, .T. ) ;
#7557 = DIRECTION ( 'NONE',  ( 0.000000000000000000, 0.000000000000000000, 1.000000000000000000 ) ) ;
#7558 = AXIS2_PLACEMENT_3D ( 'NONE', #10887, #17913, #3851 ) ;
#7559 = DIRECTION ( 'NONE',  ( 1.000000000000000000, 0.000000000000000000, 0.000000000000000000 ) ) ;
#7560 = CYLINDRICAL_SURFACE ( 'NONE', #13733, 2.844800000000091700 ) ;
#7561 = CARTESIAN_POINT ( 'NONE',  ( 76.20000000000000284, -3670.300000000000182, 2260.600000000000364 ) ) ;
#7562 = FACE_OUTER_BOUND ( 'NONE', #3515, .T. ) ;
#7563 = EDGE_LOOP ( 'NONE', ( #17629, #3166, #13129, #21802 ) ) ;
#7564 = CARTESIAN_POINT ( 'NONE',  ( 147.6473427028456342, -3695.618941227105097, 2259.780211612979656 ) ) ;
#7565 = DIRECTION ( 'NONE',  ( 0.000000000000000000, -1.000000000000000000, 0.000000000000000000 ) ) ;
#7566 = AXIS2_PLACEMENT_3D ( 'NONE', #7101, #16230, #12831 ) ;
#7567 = LINE ( 'NONE', #21866, #12571 ) ;
#7568 = EDGE_CURVE ( 'NONE', #18880, #22617, #1187, .T. ) ;
#7569 = FACE_OUTER_BOUND ( 'NONE', #22857, .T. ) ;
#7570 = CARTESIAN_POINT ( 'NONE',  ( 101.5999999999999943, -3670.300000000000182, 2259.837999999999738 ) ) ;
#7571 = CARTESIAN_POINT ( 'NONE',  ( 86.05520000000001346, -3644.899999999999636, 2259.837999999999738 ) ) ;
#7572 = ADVANCED_FACE ( 'NONE', ( #17244 ), #3303, .T. ) ;
#7573 = AXIS2_PLACEMENT_3D ( 'NONE', #12044, #19197, #22812 ) ;
#7574 = CARTESIAN_POINT ( 'NONE',  ( 7.652106483500662470, -3576.815456713399726, 2245.413922136005567 ) ) ;
#7575 = VERTEX_POINT ( 'NONE', #17592 ) ;
#7576 = PERSON_AND_ORGANIZATION_ROLE ( 'design_owner' ) ;
#7577 = VECTOR ( 'NONE', #18261, 1000.000000000000000 ) ;
#7578 = EDGE_CURVE ( 'NONE', #18291, #22051, #4872, .T. ) ;
#7579 = CARTESIAN_POINT ( 'NONE',  ( 95.25000000000000000, -3544.570000000000164, 2244.547199999999975 ) ) ;
#7580 = CARTESIAN_POINT ( 'NONE',  ( 1.270000000000000018, -3660.140000000000327, 2244.547199999999975 ) ) ;
#7581 = DIRECTION ( 'NONE',  ( 1.000000000000000000, 0.000000000000000000, 0.000000000000000000 ) ) ;
#7582 = CIRCLE ( 'NONE', #113, 5.460999999999938126 ) ;
#7583 = EDGE_CURVE ( 'NONE', #22749, #22295, #16486, .T. ) ;
#7584 = CARTESIAN_POINT ( 'NONE',  ( 55.57575231171000496, -3694.938000000000102, 2275.001800000000003 ) ) ;
#7585 = ADVANCED_FACE ( 'NONE', ( #14445 ), #5420, .T. ) ;
#7586 = CARTESIAN_POINT ( 'NONE',  ( 55.57575231171000496, -3694.938000000000102, 2275.763800000000174 ) ) ;
#7587 = EDGE_LOOP ( 'NONE', ( #3431, #21047, #19798, #4643, #7991, #20153, #8641, #320, #17586, #17699 ) ) ;
#7588 = CIRCLE ( 'NONE', #9818, 5.460999999999938126 ) ;
#7589 = DIRECTION ( 'NONE',  ( -3.194481088215918719E-14, -0.5000000000040877302, -0.8660254037820785955 ) ) ;
#7590 = CIRCLE ( 'NONE', #4230, 0.7619999999999294005 ) ;
#7591 = CARTESIAN_POINT ( 'NONE',  ( 104.4447999999999865, -3568.700000000000273, 2239.771999999999935 ) ) ;
#7592 = ORIENTED_EDGE ( 'NONE', *, *, #2430, .T. ) ;
#7593 = CARTESIAN_POINT ( 'NONE',  ( 63.50000000000000000, -3644.899999999999636, 2261.869999999999891 ) ) ;
#7594 = LINE ( 'NONE', #564, #20054 ) ;
#7595 = ORIENTED_EDGE ( 'NONE', *, *, #6952, .T. ) ;
#7596 = CARTESIAN_POINT ( 'NONE',  ( 12.69999999994000106, -3636.810100000000148, 2292.781800000000203 ) ) ;
#7597 = CARTESIAN_POINT ( 'NONE',  ( 1.270000000000000018, -3694.430000000000291, 2260.600000000000364 ) ) ;
#7598 = CIRCLE ( 'NONE', #496, 5.460999999999938126 ) ;
#7599 = ORIENTED_EDGE ( 'NONE', *, *, #6312, .F. ) ;
#7600 = CARTESIAN_POINT ( 'NONE',  ( 12.69999999999999929, -3589.528000000000247, 2262.355140000000119 ) ) ;
#7601 = UNCERTAINTY_MEASURE_WITH_UNIT (LENGTH_MEASURE( 1.000000000000000082E-05 ), #22486, 'distance_accuracy_value', 'NONE');
#7602 = ORIENTED_EDGE ( 'NONE', *, *, #16443, .T. ) ;
#7604 = CARTESIAN_POINT ( 'NONE',  ( 145.1404951596551598, -3581.245129387089946, 2245.841260533643435 ) ) ;
#7603 = VECTOR ( 'NONE', #8963, 1000.000000000000000 ) ;
#7605 = PERSON_AND_ORGANIZATION ( #5446, #1895 ) ;
#7606 = CARTESIAN_POINT ( 'NONE',  ( 64.76999999999999602, -3694.938000000000102, 2289.213099999999940 ) ) ;
#7607 = DIRECTION ( 'NONE',  ( 1.000000000000000000, 0.000000000000000000, 0.000000000000000000 ) ) ;
#7608 = DIRECTION ( 'NONE',  ( 0.000000000000000000, 0.000000000000000000, -1.000000000000000000 ) ) ;
#7609 = FACE_OUTER_BOUND ( 'NONE', #20444, .T. ) ;
#7610 = CARTESIAN_POINT ( 'NONE',  ( 141.1391456164894578, -3577.040607256482417, 2249.579133306534459 ) ) ;
#7611 = VERTEX_POINT ( 'NONE', #146 ) ;
#7612 = CIRCLE ( 'NONE', #15113, 3.606800000000000228 ) ;
#7613 = ORIENTED_EDGE ( 'NONE', *, *, #22514, .F. ) ;
#7614 = DIRECTION ( 'NONE',  ( 0.000000000000000000, 1.000000000000000000, 0.000000000000000000 ) ) ;
#7615 = EDGE_LOOP ( 'NONE', ( #10672, #7619, #22761, #2585 ) ) ;
#7616 = CARTESIAN_POINT ( 'NONE',  ( 13.32717689757000024, -3596.716669530999752, 2279.801370455999859 ) ) ;
#7617 = CARTESIAN_POINT ( 'NONE',  ( 15.54897409013627652, -3543.400907226583968, 2255.000090470922714 ) ) ;
#7618 = VECTOR ( 'NONE', #1884, 1000.000000000000000 ) ;
#7619 = ORIENTED_EDGE ( 'NONE', *, *, #3670, .T. ) ;
#7620 = CARTESIAN_POINT ( 'NONE',  ( 137.3683132029000262, -3578.148799999999937, 2242.820000000000164 ) ) ;
#7621 = CARTESIAN_POINT ( 'NONE',  ( 137.7875023037999824, -3581.600928630999988, 2246.630000000000109 ) ) ;
#7622 = ORIENTED_EDGE ( 'NONE', *, *, #337, .T. ) ;
#7623 = APPLIED_PERSON_AND_ORGANIZATION_ASSIGNMENT ( #5551, #1662, ( #2608 ) ) ;
#7624 = CARTESIAN_POINT ( 'NONE',  ( 3.048000000000000043, -3544.061999999999898, 2238.248000000000047 ) ) ;
#7625 = CARTESIAN_POINT ( 'NONE',  ( 13.65342256834697388, -3576.814163253546212, 2249.368886017665773 ) ) ;
#7626 =( NAMED_UNIT ( * ) PLANE_ANGLE_UNIT ( ) SI_UNIT ( $, .RADIAN. ) );
#7627 = DIRECTION ( 'NONE',  ( -5.461016542361937364E-28, 1.000000000000000000, -2.336881798971000105E-14 ) ) ;
#7628 = ORIENTED_EDGE ( 'NONE', *, *, #14422, .F. ) ;
#7629 = CARTESIAN_POINT ( 'NONE',  ( 64.76999999999999602, -3568.700000000000273, 2289.213099999999940 ) ) ;
#7630 = AXIS2_PLACEMENT_3D ( 'NONE', #21317, #8428, #13931 ) ;
#7631 = CALENDAR_DATE ( 2026, 26, 10 ) ;
#7632 = ADVANCED_FACE ( 'NONE', ( #19828, #12788, #1658 ), #19945, .F. ) ;
#7633 = CARTESIAN_POINT ( 'NONE',  ( 12.69999999999999929, -3584.956000000000131, 2244.978999999999814 ) ) ;
#7634 = ORIENTED_EDGE ( 'NONE', *, *, #8356, .F. ) ;
#7636 = EDGE_CURVE ( 'NONE', #20355, #15900, #18490, .T. ) ;
#7635 = CARTESIAN_POINT ( 'NONE',  ( 18.12991818266355892, -3581.277546170917049, 2245.892459010505263 ) ) ;
#7637 = ADVANCED_FACE ( 'NONE', ( #16418 ), #2016, .T. ) ;
#7638 = SPHERICAL_SURFACE ( 'NONE', #6108, 1.270000000000000018 ) ;
#7639 = VERTEX_POINT ( 'NONE', #1784 ) ;
#7640 = CARTESIAN_POINT ( 'NONE',  ( 141.4267388136501040, -3661.765907838432668, 2249.726436259035381 ) ) ;
#7641 = ADVANCED_FACE ( 'NONE', ( #7068 ), #750, .T. ) ;
#7642 = ORIENTED_EDGE ( 'NONE', *, *, #956, .F. ) ;
#7643 = CARTESIAN_POINT ( 'NONE',  ( 0.7620000000000000107, -3544.061999999999898, 2295.829799999999977 ) ) ;
#7644 = AXIS2_PLACEMENT_3D ( 'NONE', #10961, #14371, #7559 ) ;
#7645 = AXIS2_PLACEMENT_3D ( 'NONE', #13174, #4276, #20218 ) ;
#7646 = FACE_OUTER_BOUND ( 'NONE', #45, .T. ) ;
#7647 = AXIS2_PLACEMENT_3D ( 'NONE', #5709, #5597, #5479 ) ;
#7648 = EDGE_LOOP ( 'NONE', ( #16356, #8002, #14497, #13722 ) ) ;
#7649 = DIRECTION ( 'NONE',  ( 1.000000000000000000, 0.000000000000000000, 0.000000000000000000 ) ) ;
#7650 = DIRECTION ( 'NONE',  ( 0.000000000000000000, 1.000000000000000000, 0.000000000000000000 ) ) ;
#7651 = ORIENTED_EDGE ( 'NONE', *, *, #22596, .T. ) ;
#7652 = DIRECTION ( 'NONE',  ( 0.000000000000000000, 0.000000000000000000, -1.000000000000000000 ) ) ;
#7653 = FACE_BOUND ( 'NONE', #16045, .T. ) ;
#7654 = CARTESIAN_POINT ( 'NONE',  ( 7.179586105935542584, -3580.969250050631217, 2245.481136081417844 ) ) ;
#7655 = CARTESIAN_POINT ( 'NONE',  ( 63.50000000000000000, -3594.099999999999909, 2239.771999999999935 ) ) ;
#7656 = COORDINATED_UNIVERSAL_TIME_OFFSET ( 0, 0, .AHEAD. ) ;
#7657 = EDGE_CURVE ( 'NONE', #15883, #8860, #16842, .T. ) ;
#7658 = CARTESIAN_POINT ( 'NONE',  ( 25.98329380356999962, -3544.061999999999898, 2247.650964417000068 ) ) ;
#7659 = VECTOR ( 'NONE', #8492, 1000.000000000000000 ) ;
#7660 = AXIS2_PLACEMENT_3D ( 'NONE', #21801, #14549, #2464 ) ;
#7661 = EDGE_CURVE ( 'NONE', #19085, #3900, #15367, .T. ) ;
#7663 = ADVANCED_FACE ( 'NONE', ( #12906 ), #3418, .T. ) ;
#7662 = CIRCLE ( 'NONE', #14401, 0.7620000000000366480 ) ;
#7665 = CARTESIAN_POINT ( 'NONE',  ( 142.4715777200796367, -3658.856899883896403, 2249.932665716038628 ) ) ;
#7664 = APPLICATION_CONTEXT ( 'configuration controlled 3d designs of mechanical parts and assemblies' ) ;
#7666 = CARTESIAN_POINT ( 'NONE',  ( 12.69999999999999929, -3659.504999999999654, 2270.760000000000218 ) ) ;
#7667 = AXIS2_PLACEMENT_3D ( 'NONE', #15989, #4029, #5679 ) ;
#7668 = ORIENTED_EDGE ( 'NONE', *, *, #5162, .T. ) ;
#7669 = CARTESIAN_POINT ( 'NONE',  ( -5.588000000000000078, -3660.140000000000327, 2243.785200000000259 ) ) ;
#7670 = DIRECTION ( 'NONE',  ( -1.000000000000000000, 0.000000000000000000, 0.000000000000000000 ) ) ;
#7671 = ADVANCED_BREP_SHAPE_REPRESENTATION ( '', ( #13285, #5611 ), #15735 ) ;
#7672 = CARTESIAN_POINT ( 'NONE',  ( 12.69999999999999929, -3653.789999999999964, 2268.705139999999574 ) ) ;
#7673 = CARTESIAN_POINT ( 'NONE',  ( 0.000000000000000000, -3660.140000000000327, 2247.392000000000280 ) ) ;
#7674 = ORIENTED_EDGE ( 'NONE', *, *, #9106, .F. ) ;
#7675 = CARTESIAN_POINT ( 'NONE',  ( 147.5973730189926982, -3543.437357047961086, 2259.905208148476504 ) ) ;
#7676 = ORIENTED_EDGE ( 'NONE', *, *, #6510, .F. ) ;
#7677 = CARTESIAN_POINT ( 'NONE',  ( 15.54479972196000048, -3659.504985917999875, 2257.962943248000101 ) ) ;
#7678 = ADVANCED_FACE ( 'NONE', ( #17709 ), #16074, .T. ) ;
#7679 = CIRCLE ( 'NONE', #10673, 5.460999999999938126 ) ;
#7680 = DIRECTION ( 'NONE',  ( 1.000000000000000000, 1.206643234470999950E-12, 0.000000000000000000 ) ) ;
#7681 = VECTOR ( 'NONE', #13351, 1000.000000000000000 ) ;
#7682 = DIRECTION ( 'NONE',  ( 2.336881798971000105E-14, 0.000000000000000000, 1.000000000000000000 ) ) ;
#7683 = TOROIDAL_SURFACE ( 'NONE', #9909, 6.477000000000000313, 0.7620000000000000107 ) ;
#7684 = CARTESIAN_POINT ( 'NONE',  ( 12.69999999999999929, -3579.494999999999891, 2239.009999999999764 ) ) ;
#7685 = CIRCLE ( 'NONE', #9183, 1.904999999999823501 ) ;
#7686 = DIRECTION ( 'NONE',  ( 0.000000000000000000, 1.000000000000000000, 0.000000000000000000 ) ) ;
#7687 = DIRECTION ( 'NONE',  ( 2.336881798971000105E-14, 0.000000000000000000, 1.000000000000000000 ) ) ;
#7688 = CARTESIAN_POINT ( 'NONE',  ( 7.020348529275000082, -3578.860230781999689, 2244.548186305999934 ) ) ;
#7689 = EDGE_LOOP ( 'NONE', ( #17633, #17679, #8543, #17164 ) ) ;
#7690 = COORDINATED_UNIVERSAL_TIME_OFFSET ( 0, 0, .AHEAD. ) ;
#7691 = CARTESIAN_POINT ( 'NONE',  ( 145.1681434097811234, -3657.843844258350600, 2245.707489631754015 ) ) ;
#7692 = CARTESIAN_POINT ( 'NONE',  ( 15.24000000000000021, -3660.786127253999894, 2255.774000000000342 ) ) ;
#7693 = DIRECTION ( 'NONE',  ( -7.280632624815000075E-13, -1.000000000000000000, -3.793660610169000352E-12 ) ) ;
#7694 = AXIS2_PLACEMENT_3D ( 'NONE', #4646, #10037, #17180 ) ;
#7695 = ORIENTED_EDGE ( 'NONE', *, *, #14636, .T. ) ;
#7696 = CIRCLE ( 'NONE', #8460, 5.460999999999938126 ) ;
#7697 = CARTESIAN_POINT ( 'NONE',  ( 25.39999999999999858, -3670.300000000000182, 2259.837999999999738 ) ) ;
#7698 = EDGE_CURVE ( 'NONE', #4281, #18582, #3383, .T. ) ;
#7699 = APPLICATION_CONTEXT ( 'configuration controlled 3d designs of mechanical parts and assemblies' ) ;
#7700 = TOROIDAL_SURFACE ( 'NONE', #22285, 5.080000000000000071, 0.3810000000000000053 ) ;
#7701 = EDGE_CURVE ( 'NONE', #3136, #6642, #20438, .T. ) ;
#7702 = CIRCLE ( 'NONE', #17750, 5.714999999998999769 ) ;
#7703 = EDGE_CURVE ( 'NONE', #22988, #10080, #9383, .T. ) ;
#7704 = ORIENTED_EDGE ( 'NONE', *, *, #21194, .F. ) ;
#7705 = DIRECTION ( 'NONE',  ( -1.000000000000000000, 0.000000000000000000, 0.000000000000000000 ) ) ;
#7706 = VERTEX_POINT ( 'NONE', #1601 ) ;
#7707 = CIRCLE ( 'NONE', #6599, 5.460999999999938126 ) ;
#7708 = CARTESIAN_POINT ( 'NONE',  ( 14.51618957457999493, -3661.694864241059349, 2249.774377504978474 ) ) ;
#7709 = DIRECTION ( 'NONE',  ( -1.000000000000000000, 0.000000000000000000, 0.000000000000000000 ) ) ;
#7710 = ORIENTED_EDGE ( 'NONE', *, *, #14422, .T. ) ;
#7711 = ADVANCED_FACE ( 'NONE', ( #8206 ), #5246, .F. ) ;
#7712 = CARTESIAN_POINT ( 'NONE',  ( 9.653930614662758813, -3657.399154393335721, 2246.629994487922431 ) ) ;
#7713 = CARTESIAN_POINT ( 'NONE',  ( 139.7000000000001876, -3662.679999999999836, 2245.359999999999673 ) ) ;
#7714 = ORIENTED_EDGE ( 'NONE', *, *, #9565, .F. ) ;
#7715 = DIRECTION ( 'NONE',  ( 0.000000000000000000, 0.000000000000000000, 1.000000000000000000 ) ) ;
#7716 = AXIS2_PLACEMENT_3D ( 'NONE', #15527, #12478, #21387 ) ;
#7717 = DIRECTION ( 'NONE',  ( 0.000000000000000000, 0.000000000000000000, -1.000000000000000000 ) ) ;
#7718 = ORIENTED_EDGE ( 'NONE', *, *, #1509, .T. ) ;
#7719 = AXIS2_PLACEMENT_3D ( 'NONE', #15990, #1686, #17620 ) ;
#7720 = VECTOR ( 'NONE', #15511, 1000.000000000000000 ) ;
#7721 = EDGE_CURVE ( 'NONE', #2758, #8066, #3764, .T. ) ;
#7722 = VERTEX_POINT ( 'NONE', #23149 ) ;
#7723 = PRODUCT_DEFINITION_SHAPE ( 'NONE', 'NONE',  #23172 ) ;
#7724 = AXIS2_PLACEMENT_3D ( 'NONE', #11893, #2980, #13774 ) ;
#7725 = ADVANCED_FACE ( 'NONE', ( #22485 ), #9013, .T. ) ;
#7726 = CARTESIAN_POINT ( 'NONE',  ( 66.34479999999999222, -3644.899999999999636, 2239.771999999999935 ) ) ;
#7727 = ORIENTED_EDGE ( 'NONE', *, *, #17551, .T. ) ;
#7728 = B_SPLINE_CURVE_WITH_KNOTS ( 'NONE', 3,
 ( #18143, #7483, #16276, #19677, #3966, #7041, #11123, #21438, #12646, #5743, #9251, #14641, #21668, #7376, #1863, #19796, #12759, #16389, #9134, #14292, #14529, #14407, #18260, #9362, #12528, #5623, #21783, #19913, #111, #3850, #14183 ),
 .UNSPECIFIED., .F., .F.,
 ( 4, 2, 2, 2, 2, 2, 1, 2, 2, 2, 2, 1, 1, 2, 2, 2, 4 ),
 ( 0.000000000000000000, 0.1250000000011337598, 0.1875000000020345392, 0.2500000000029353187, 0.3750000000047304383, 0.4375000000053519411, 0.4687500000056163962, 0.4843750000059510175, 0.5000000000062856387, 0.6250000000045987658, 0.6875000000039348524, 0.7187500000033559822, 0.7343750000030726532, 0.7421875000030454528, 0.7500000000030181413, 0.8750000000015091262, 1.000000000000000000 ),
 .UNSPECIFIED. ) ;
#7729 = DIRECTION ( 'NONE',  ( 1.000000000000000000, 0.000000000000000000, 0.000000000000000000 ) ) ;
#7730 = SHAPE_REPRESENTATION ( 'Base Plate', ( #5611 ), #2239 ) ;
#7731 = AXIS2_PLACEMENT_3D ( 'NONE', #23022, #5465, #17991 ) ;
#7732 = SHAPE_DEFINITION_REPRESENTATION ( #20441, #6985 ) ;
#7733 = CIRCLE ( 'NONE', #20822, 2.844800000000091700 ) ;
#7734 = CARTESIAN_POINT ( 'NONE',  ( 18.34030854049733605, -3660.434275077790517, 2244.558523461154437 ) ) ;
#7735 = CARTESIAN_POINT ( 'NONE',  ( 21.79320000000099711, -3670.300000000000182, 2239.771999999999935 ) ) ;
#7736 = CARTESIAN_POINT ( 'NONE',  ( 11.36482343738000012, -3576.977758867000375, 2257.672197237000091 ) ) ;
#7737 = EDGE_CURVE ( 'NONE', #8199, #12626, #12757, .T. ) ;
#7738 = CARTESIAN_POINT ( 'NONE',  ( 142.0475659686787822, -3577.885968673145271, 2250.065841773341617 ) ) ;
#7739 = ORIENTED_EDGE ( 'NONE', *, *, #4489, .T. ) ;
#7740 = AXIS2_PLACEMENT_3D ( 'NONE', #61, #12822, #20206 ) ;
#7741 = ORIENTED_EDGE ( 'NONE', *, *, #3342, .T. ) ;
#7742 = DIRECTION ( 'NONE',  ( 0.000000000000000000, 0.000000000000000000, 1.000000000000000000 ) ) ;
#7743 = VERTEX_POINT ( 'NONE', #22601 ) ;
#7744 = DIRECTION ( 'NONE',  ( -1.000000000000000000, 0.000000000000000000, 0.000000000000000000 ) ) ;
#7745 = AXIS2_PLACEMENT_3D ( 'NONE', #18721, #2671, #4899 ) ;
#7746 = CARTESIAN_POINT ( 'NONE',  ( 1.270000000000000018, -3544.570000000000164, 2240.279999999999745 ) ) ;
#7747 = AXIS2_PLACEMENT_3D ( 'NONE', #9209, #18561, #16688 ) ;
#7748 = EDGE_LOOP ( 'NONE', ( #1419, #22998, #11862, #19788 ) ) ;
#7749 = AXIS2_PLACEMENT_3D ( 'NONE', #17287, #15544, #5001 ) ;
#7750 = ORIENTED_EDGE ( 'NONE', *, *, #10002, .F. ) ;
#7751 = B_SPLINE_CURVE_WITH_KNOTS ( 'NONE', 3,
 ( #9898, #876, #1230, #16819 ),
 .UNSPECIFIED., .F., .F.,
 ( 4, 4 ),
 ( 0.000000000000000000, 1.000000000000000000 ),
 .UNSPECIFIED. ) ;
#7752 = ORIENTED_EDGE ( 'NONE', *, *, #7798, .F. ) ;
#7753 = LINE ( 'NONE', #813, #19693 ) ;
#7754 = CARTESIAN_POINT ( 'NONE',  ( 13.59572439041964032, -3576.794808590030243, 2249.348515776098338 ) ) ;
#7755 = DIRECTION ( 'NONE',  ( -5.197384013923000042E-14, -1.000000000000000000, 2.639941086436999774E-14 ) ) ;
#7756 = ORIENTED_EDGE ( 'NONE', *, *, #2760, .F. ) ;
#7757 = CIRCLE ( 'NONE', #16729, 2.844800000000098361 ) ;
#7758 = CARTESIAN_POINT ( 'NONE',  ( 136.8737850040470505, -3659.879057353201461, 2257.957974146814649 ) ) ;
#7759 = PERSON_AND_ORGANIZATION_ROLE ( 'creator' ) ;
#7760 = CIRCLE ( 'NONE', #7391, 4.114799999999974034 ) ;
#7761 = DIRECTION ( 'NONE',  ( 0.000000000000000000, 0.000000000000000000, 1.000000000000000000 ) ) ;
#7762 = CARTESIAN_POINT ( 'NONE',  ( -12.54218463262943217, -3580.206200000482568, 2245.060313202995985 ) ) ;
#7763 = CARTESIAN_POINT ( 'NONE',  ( 35.56000000000000227, -3670.300000000000182, 2247.392000000000280 ) ) ;
#7764 = AXIS2_PLACEMENT_3D ( 'NONE', #6300, #19055, #11656 ) ;
#7765 = AXIS2_PLACEMENT_3D ( 'NONE', #10579, #5426, #17715 ) ;
#7766 = AXIS2_PLACEMENT_3D ( 'NONE', #16308, #19944, #20173 ) ;
#7767 = ORIENTED_EDGE ( 'NONE', *, *, #20824, .T. ) ;
#7768 = CARTESIAN_POINT ( 'NONE',  ( 141.8096541925104077, -3661.413627425323284, 2249.935838938367851 ) ) ;
#7769 = APPLIED_PERSON_AND_ORGANIZATION_ASSIGNMENT ( #14791, #3888, ( #4122 ) ) ;
#7770 = ORIENTED_EDGE ( 'NONE', *, *, #8941, .T. ) ;
#7771 = ORIENTED_EDGE ( 'NONE', *, *, #18279, .T. ) ;
#7772 = AXIS2_PLACEMENT_3D ( 'NONE', #12534, #241, #23070 ) ;
#7773 = CARTESIAN_POINT ( 'NONE',  ( 15.03168679713838074, -3600.843700000154968, 2296.433984632765259 ) ) ;
#7774 = EDGE_CURVE ( 'NONE', #17371, #17962, #14639, .T. ) ;
#7775 = EDGE_LOOP ( 'NONE', ( #647, #6157 ) ) ;
#7776 = CARTESIAN_POINT ( 'NONE',  ( 25.39999999999999858, -3568.700000000000273, 2239.771999999999935 ) ) ;
#7777 = CARTESIAN_POINT ( 'NONE',  ( 1.048684632737000300, -3544.061999999999898, 2273.953115367000009 ) ) ;
#7778 = EDGE_LOOP ( 'NONE', ( #5318, #22918, #13917, #6937 ) ) ;
#7779 = VECTOR ( 'NONE', #1763, 999.9999999999998863 ) ;
#7780 = CARTESIAN_POINT ( 'NONE',  ( 7.223429647927347652, -3657.870544957902439, 2245.674539183268280 ) ) ;
#7781 = DIRECTION ( 'NONE',  ( 0.000000000000000000, -1.000000000000000000, 0.000000000000000000 ) ) ;
#7782 = DIRECTION ( 'NONE',  ( 0.000000000000000000, 0.000000000000000000, -1.000000000000000000 ) ) ;
#7783 = CARTESIAN_POINT ( 'NONE',  ( 129.8447999999989975, -3568.700000000000273, 2239.771999999999935 ) ) ;
#7784 = COORDINATED_UNIVERSAL_TIME_OFFSET ( 0, 0, .AHEAD. ) ;
#7785 = DIRECTION ( 'NONE',  ( 0.000000000000000000, -1.000000000000000000, 0.000000000000000000 ) ) ;
#7786 = ORIENTED_EDGE ( 'NONE', *, *, #22096, .F. ) ;
#7787 = CARTESIAN_POINT ( 'NONE',  ( 12.69999999999999929, -3653.789999999999964, 2274.293139999999767 ) ) ;
#7788 = CIRCLE ( 'NONE', #9282, 4.114799999999974034 ) ;
#7789 = CARTESIAN_POINT ( 'NONE',  ( 127.0000000000000000, -3660.140000000000327, 2247.392000000000280 ) ) ;
#7790 = ORIENTED_EDGE ( 'NONE', *, *, #21135, .F. ) ;
#7791 = CARTESIAN_POINT ( 'NONE',  ( 139.6999999999999886, -3659.504999999999654, 2239.009999999999764 ) ) ;
#7792 = APPLIED_PERSON_AND_ORGANIZATION_ASSIGNMENT ( #5040, #7576, ( #5080 ) ) ;
#7793 = DIRECTION ( 'NONE',  ( 0.5000000000031612490, -0.8660254037826135010, 0.000000000000000000 ) ) ;
#7794 = VERTEX_POINT ( 'NONE', #6577 ) ;
#7795 = DIRECTION ( 'NONE',  ( 0.000000000000000000, 1.000000000000000000, 0.000000000000000000 ) ) ;
#7796 = EDGE_LOOP ( 'NONE', ( #16489, #10920, #12529, #8960 ) ) ;
#7797 = CARTESIAN_POINT ( 'NONE',  ( 15.03168679714000078, -3638.156300000000101, 2292.781800000000203 ) ) ;
#7798 = EDGE_CURVE ( 'NONE', #1742, #13263, #414, .T. ) ;
#7799 = ORIENTED_EDGE ( 'NONE', *, *, #23017, .T. ) ;
#7800 = ORIENTED_EDGE ( 'NONE', *, *, #269, .F. ) ;
#7801 = DIRECTION ( 'NONE',  ( 0.000000000000000000, 0.000000000000000000, 1.000000000000000000 ) ) ;
#7802 = EDGE_CURVE ( 'NONE', #15650, #15285, #22095, .T. ) ;
#7803 = CARTESIAN_POINT ( 'NONE',  ( 137.3683132029000262, -3580.841199999999844, 2239.391000000000076 ) ) ;
#7804 = DIRECTION ( 'NONE',  ( -0.5000000000047110094, -0.8660254037817188832, 0.000000000000000000 ) ) ;
#7805 = EDGE_CURVE ( 'NONE', #11209, #8599, #15000, .T. ) ;
#7806 = CARTESIAN_POINT ( 'NONE',  ( -5.588000000000000078, -3694.938000000000102, 2229.612000000000080 ) ) ;
#7807 = DIRECTION ( 'NONE',  ( 0.000000000000000000, -1.000000000000000000, 0.000000000000000000 ) ) ;
#7808 = DIRECTION ( 'NONE',  ( 0.5000000000047110094, -0.8660254037817188832, 0.000000000000000000 ) ) ;
#7809 = DIRECTION ( 'NONE',  ( 0.000000000000000000, 0.000000000000000000, 1.000000000000000000 ) ) ;
#7810 = VERTEX_POINT ( 'NONE', #12503 ) ;
#7811 = APPROVAL_STATUS ( 'not_yet_approved' ) ;
#7812 = CARTESIAN_POINT ( 'NONE',  ( 54.40679999999999694, -3619.500000000000000, 2239.771999999999935 ) ) ;
#7813 = EDGE_CURVE ( 'NONE', #20661, #8067, #10987, .T. ) ;
#7814 = FACE_OUTER_BOUND ( 'NONE', #21871, .T. ) ;
#7815 = CARTESIAN_POINT ( 'NONE',  ( 25.39999999999999858, -3578.860000000000127, 2250.236800000000130 ) ) ;
#7816 = EDGE_CURVE ( 'NONE', #2568, #7197, #8880, .T. ) ;
#7817 = VERTEX_POINT ( 'NONE', #14272 ) ;
#7818 = DIRECTION ( 'NONE',  ( 0.000000000000000000, -1.000000000000000000, 0.000000000000000000 ) ) ;
#7819 = DIRECTION ( 'NONE',  ( 1.000000000000000000, 0.000000000000000000, 0.000000000000000000 ) ) ;
#7820 = ORIENTED_EDGE ( 'NONE', *, *, #2424, .T. ) ;
#7821 = AXIS2_PLACEMENT_3D ( 'NONE', #9074, #17974, #19742 ) ;
#7822 = DIRECTION ( 'NONE',  ( -1.000000000000000000, 1.224646799147353207E-16, 0.000000000000000000 ) ) ;
#7823 = CARTESIAN_POINT ( 'NONE',  ( 14.97732264284127446, -3661.210416770012216, 2250.027943346653501 ) ) ;
#7824 = DIRECTION ( 'NONE',  ( 0.000000000000000000, -1.000000000000000000, 0.000000000000000000 ) ) ;
#7825 = ORIENTED_EDGE ( 'NONE', *, *, #988, .T. ) ;
#7826 = DIRECTION ( 'NONE',  ( 0.000000000000000000, 0.000000000000000000, 1.000000000000000000 ) ) ;
#7827 = EDGE_CURVE ( 'NONE', #11664, #10874, #6878, .T. ) ;
#7828 = ORIENTED_EDGE ( 'NONE', *, *, #11880, .F. ) ;
#7829 = DIRECTION ( 'NONE',  ( 0.000000000000000000, 0.000000000000000000, -1.000000000000000000 ) ) ;
#7830 = FACE_OUTER_BOUND ( 'NONE', #3015, .T. ) ;
#7831 = EDGE_LOOP ( 'NONE', ( #18424, #7367, #4071, #6367 ) ) ;
#7832 = ORIENTED_EDGE ( 'NONE', *, *, #4227, .T. ) ;
#7833 = VECTOR ( 'NONE', #2992, 1000.000000000000000 ) ;
#7834 = EDGE_CURVE ( 'NONE', #6249, #1742, #17714, .T. ) ;
#7835 = EDGE_CURVE ( 'NONE', #4963, #8499, #15099, .T. ) ;
#7836 = DIRECTION ( 'NONE',  ( 1.000000000000000000, 0.000000000000000000, 0.000000000000000000 ) ) ;
#7837 = UNCERTAINTY_MEASURE_WITH_UNIT (LENGTH_MEASURE( 1.000000000000000082E-05 ), #5801, 'distance_accuracy_value', 'NONE');
#7838 = EDGE_LOOP ( 'NONE', ( #17049, #3505, #8526, #8471 ) ) ;
#7839 = AXIS2_PLACEMENT_3D ( 'NONE', #7684, #18462, #9671 ) ;
#7840 = DIRECTION ( 'NONE',  ( 0.000000000000000000, 0.8660254037838039931, 0.5000000000010993428 ) ) ;
#7841 = PRODUCT_CONTEXT ( 'NONE', #19647, 'mechanical' ) ;
#7842 = CARTESIAN_POINT ( 'NONE',  ( 12.69999999999999929, -3642.347301254450485, 2279.817638608977632 ) ) ;
#7843 = CARTESIAN_POINT ( 'NONE',  ( 17.44548393074270365, -3662.697233759483879, 2246.100251725204544 ) ) ;
#7844 = CARTESIAN_POINT ( 'NONE',  ( 131.8733692468000243, -3544.443975433000105, 2260.595783961000052 ) ) ;
#7845 = DIRECTION ( 'NONE',  ( 1.224646799147353207E-16, 1.000000000000000000, -0.000000000000000000 ) ) ;
#7846 = LINE ( 'NONE', #17083, #8390 ) ;
#7847 = ORIENTED_EDGE ( 'NONE', *, *, #4726, .F. ) ;
#7848 = EDGE_CURVE ( 'NONE', #8227, #861, #2305, .T. ) ;
#7849 = AXIS2_PLACEMENT_3D ( 'NONE', #9024, #16286, #21570 ) ;
#7850 = LINE ( 'NONE', #13349, #11846 ) ;
#7851 = CARTESIAN_POINT ( 'NONE',  ( 10.21049783553828050, -3598.060185255057604, 2296.591800000037438 ) ) ;
#7852 = ORIENTED_EDGE ( 'NONE', *, *, #1235, .F. ) ;
#7853 = APPLIED_APPROVAL_ASSIGNMENT ( #3045, ( #9636 ) ) ;
#7854 = CARTESIAN_POINT ( 'NONE',  ( 15.27310946263999902, -3598.270206608000080, 2279.515940941999816 ) ) ;
#7855 = VECTOR ( 'NONE', #2043, 1000.000000000000000 ) ;
#7856 = CARTESIAN_POINT ( 'NONE',  ( 12.69999999999999929, -3639.502500000000055, 2264.841800000000148 ) ) ;
#7857 = ORIENTED_EDGE ( 'NONE', *, *, #11693, .F. ) ;
#7858 = VERTEX_POINT ( 'NONE', #16593 ) ;
#7859 = ORIENTED_EDGE ( 'NONE', *, *, #18021, .T. ) ;
#7860 = FACE_OUTER_BOUND ( 'NONE', #20161, .T. ) ;
#7861 =( BOUNDED_CURVE ( )  B_SPLINE_CURVE ( 3, ( #6513, #20794, #10128, #18919 ),
 .UNSPECIFIED., .F., .T. ) 
 B_SPLINE_CURVE_WITH_KNOTS ( ( 4, 4 ),
 ( -2.664535259100375697E-14, 1.570796326277596799 ),
 .UNSPECIFIED. ) 
 CURVE ( )  GEOMETRIC_REPRESENTATION_ITEM ( )  RATIONAL_B_SPLINE_CURVE ( ( 1.000000000000000000, 0.8047378542462874096, 0.8047378542462874096, 1.000000000000000000 ) ) 
 REPRESENTATION_ITEM ( '' )  );
#7862 = VERTEX_POINT ( 'NONE', #14616 ) ;
#7863 = LINE ( 'NONE', #5996, #20433 ) ;
#7864 = EDGE_CURVE ( 'NONE', #7722, #7479, #9452, .T. ) ;
#7865 = CARTESIAN_POINT ( 'NONE',  ( 14.89507094893205519, -3577.685273219328337, 2249.982988182303870 ) ) ;
#7866 =( LENGTH_UNIT ( ) NAMED_UNIT ( * ) SI_UNIT ( .MILLI., .METRE. ) );
#7867 = CARTESIAN_POINT ( 'NONE',  ( 141.8137592268451499, -3581.398919698233840, 2248.675269099207981 ) ) ;
#7868 = VERTEX_POINT ( 'NONE', #3824 ) ;
#7869 = CARTESIAN_POINT ( 'NONE',  ( 136.8552000000009912, -3659.504999999999654, 2257.962944264955240 ) ) ;
#7870 = DATE_AND_TIME ( #6002, #20215 ) ;
#7871 = DIRECTION ( 'NONE',  ( 1.000000000000000000, 0.000000000000000000, 0.000000000000000000 ) ) ;
#7872 = LOCAL_TIME ( 17, 37, 43.00000000000000000, #21903 ) ;
#7873 = DIRECTION ( 'NONE',  ( -1.000000000000000000, 0.000000000000000000, 0.000000000000000000 ) ) ;
#7874 = AXIS2_PLACEMENT_3D ( 'NONE', #8207, #13599, #22372 ) ;
#7875 = CARTESIAN_POINT ( 'NONE',  ( 138.9614758940914214, -3576.741457189147241, 2257.615706727020552 ) ) ;
#7876 = ORIENTED_EDGE ( 'NONE', *, *, #6379, .F. ) ;
#7877 = ADVANCED_FACE ( 'NONE', ( #18234 ), #2736, .T. ) ;
#7878 = DIRECTION ( 'NONE',  ( 1.000000000000000000, 0.000000000000000000, 0.000000000000000000 ) ) ;
#7879 = EDGE_CURVE ( 'NONE', #4712, #3136, #542, .T. ) ;
#7880 = VERTEX_POINT ( 'NONE', #12970 ) ;
#7881 = VERTEX_POINT ( 'NONE', #21758 ) ;
#7882 = DIRECTION ( 'NONE',  ( -1.000000000000000000, 0.000000000000000000, 0.000000000000000000 ) ) ;
#7883 = CIRCLE ( 'NONE', #20983, 1.904999999999823501 ) ;
#7884 = CARTESIAN_POINT ( 'NONE',  ( 12.69999999999999929, -3659.504999999999654, 2239.771999999999935 ) ) ;
#7885 = ORIENTED_EDGE ( 'NONE', *, *, #1108, .T. ) ;
#7886 = LOCAL_TIME ( 17, 37, 43.00000000000000000, #13951 ) ;
#7887 = DIRECTION ( 'NONE',  ( 0.000000000000000000, -1.000000000000000000, 0.000000000000000000 ) ) ;
#7888 = CARTESIAN_POINT ( 'NONE',  ( 35.56000000000000227, -3568.700000000000273, 2247.392000000000280 ) ) ;
#7889 = APPLIED_APPROVAL_ASSIGNMENT ( #12657, ( #14623 ) ) ;
#7890 = VERTEX_POINT ( 'NONE', #5834 ) ;
#7891 = CARTESIAN_POINT ( 'NONE',  ( 7.155628190510333830, -3658.118427763718046, 2245.389413767294627 ) ) ;
#7892 = CARTESIAN_POINT ( 'NONE',  ( 152.4000000000000057, -3695.699999999999818, 2239.009999999999764 ) ) ;
#7893 = LINE ( 'NONE', #1074, #19960 ) ;
#7894 = CARTESIAN_POINT ( 'NONE',  ( 12.69999999999999929, -3639.502500000000055, 2296.591799999999694 ) ) ;
#7895 = CALENDAR_DATE ( 2026, 26, 10 ) ;
#7896 = VECTOR ( 'NONE', #14949, 1000.000000000000000 ) ;
#7897 = FACE_OUTER_BOUND ( 'NONE', #18768, .T. ) ;
#7898 = CARTESIAN_POINT ( 'NONE',  ( 142.5447969220999767, -3659.505006299999877, 2250.165025787000104 ) ) ;
#7899 = FACE_BOUND ( 'NONE', #16294, .T. ) ;
#7900 = LOCAL_TIME ( 17, 37, 43.00000000000000000, #2086 ) ;
#7901 = LOCAL_TIME ( 17, 37, 43.00000000000000000, #21040 ) ;
#7902 = ORIENTED_EDGE ( 'NONE', *, *, #12219, .T. ) ;
#7903 = CARTESIAN_POINT ( 'NONE',  ( 137.0705190374700351, -3543.848287276122392, 2255.549776698934238 ) ) ;
#7904 = DIRECTION ( 'NONE',  ( 1.000000000000000000, 0.000000000000000000, 0.000000000000000000 ) ) ;
#7905 = ORIENTED_EDGE ( 'NONE', *, *, #2098, .T. ) ;
#7906 = CARTESIAN_POINT ( 'NONE',  ( 139.6999999999999886, -3582.187399999999798, 2242.820000000000164 ) ) ;
#7907 = PRODUCT_DEFINITION_SHAPE ( 'NONE', 'NONE',  #23170 ) ;
#7908 = AXIS2_PLACEMENT_3D ( 'NONE', #954, #15037, #4590 ) ;
#7909 = CARTESIAN_POINT ( 'NONE',  ( 9.987313202862001305, -3659.504999999999654, 2239.391000000000076 ) ) ;
#7910 = ORIENTED_EDGE ( 'NONE', *, *, #21752, .T. ) ;
#7911 = EDGE_LOOP ( 'NONE', ( #8852, #17855, #14794, #22893, #15404, #5877, #3733, #5210, #22182, #7710 ) ) ;
#7912 = DIRECTION ( 'NONE',  ( 1.000000000000000000, 0.000000000000000000, 0.000000000000000000 ) ) ;
#7913 = CARTESIAN_POINT ( 'NONE',  ( 127.0000000000000000, -3578.860000000000127, 2250.236800000000130 ) ) ;
#7914 = DIRECTION ( 'NONE',  ( 0.000000000000000000, 0.000000000000000000, 1.000000000000000000 ) ) ;
#7915 = DIRECTION ( 'NONE',  ( 0.000000000000000000, 0.000000000000000000, 1.000000000000000000 ) ) ;
#7916 = CARTESIAN_POINT ( 'NONE',  ( 25.39999999999999858, -3568.700000000000273, 2239.771999999999935 ) ) ;
#7917 = DIRECTION ( 'NONE',  ( 0.000000000000000000, 1.000000000000000000, 0.000000000000000000 ) ) ;
#7918 = CARTESIAN_POINT ( 'NONE',  ( 20.66691620702998478, -3695.635001937071593, 2259.731083289085291 ) ) ;
#7919 = EDGE_LOOP ( 'NONE', ( #6190, #11906 ) ) ;
#7920 = PERSON_AND_ORGANIZATION_ROLE ( 'creator' ) ;
#7921 = APPROVAL ( #19482, 'UNSPECIFIED' ) ;
#7922 = CARTESIAN_POINT ( 'NONE',  ( 12.69999999999999929, -3574.034000000000106, 2245.359999999999673 ) ) ;
#7923 = AXIS2_PLACEMENT_3D ( 'NONE', #5554, #16200, #2023 ) ;
#7924 = CIRCLE ( 'NONE', #3437, 5.714999999999999858 ) ;
#7925 = LINE ( 'NONE', #6065, #15064 ) ;
#7926 = EDGE_CURVE ( 'NONE', #20430, #16634, #6758, .T. ) ;
#7927 = CARTESIAN_POINT ( 'NONE',  ( 131.7757523116999891, -3544.570000000000164, 2260.600000000000364 ) ) ;
#7928 = EDGE_CURVE ( 'NONE', #16884, #3779, #993, .T. ) ;
#7929 = VERTEX_POINT ( 'NONE', #20674 ) ;
#7930 = CARTESIAN_POINT ( 'NONE',  ( 12.69999999999999929, -3644.963499999999840, 2290.241799999999785 ) ) ;
#7931 = EDGE_CURVE ( 'NONE', #22749, #19266, #21844, .T. ) ;
#7932 = ORIENTED_EDGE ( 'NONE', *, *, #9962, .F. ) ;
#7933 = DIRECTION ( 'NONE',  ( 0.000000000000000000, 1.000000000000000000, 0.000000000000000000 ) ) ;
#7934 = CARTESIAN_POINT ( 'NONE',  ( 134.2179335353430076, -3577.879693976099134, 2244.721041474473623 ) ) ;
#7935 = ORIENTED_EDGE ( 'NONE', *, *, #3283, .T. ) ;
#7936 = CARTESIAN_POINT ( 'NONE',  ( 12.69999999999143903, -3602.372129489641338, 2296.591799999931936 ) ) ;
#7937 = CIRCLE ( 'NONE', #21038, 1.269999999999882334 ) ;
#7938 = DIRECTION ( 'NONE',  ( 0.000000000000000000, -1.000000000000000000, 0.000000000000000000 ) ) ;
#7939 = LINE ( 'NONE', #9910, #235 ) ;
#7940 = VERTEX_POINT ( 'NONE', #4403 ) ;
#7941 = EDGE_CURVE ( 'NONE', #767, #19446, #1622, .T. ) ;
#7942 = AXIS2_PLACEMENT_3D ( 'NONE', #10802, #9045, #16646 ) ;
#7943 = CARTESIAN_POINT ( 'NONE',  ( 12.69999999999999929, -3648.710000000000036, 2268.705139999999574 ) ) ;
#7944 = CIRCLE ( 'NONE', #21045, 11.11250000000000071 ) ;
#7945 = FACE_OUTER_BOUND ( 'NONE', #20148, .T. ) ;
#7946 = VECTOR ( 'NONE', #21587, 1000.000000000000000 ) ;
#7947 = DIRECTION ( 'NONE',  ( 0.000000000000000000, 0.000000000000000000, -1.000000000000000000 ) ) ;
#7948 = CARTESIAN_POINT ( 'NONE',  ( 9.855199999999999960, -3659.504999999999654, 2272.030000000000200 ) ) ;
#7949 = EDGE_CURVE ( 'NONE', #22852, #12409, #20718, .T. ) ;
#7950 = ORIENTED_EDGE ( 'NONE', *, *, #776, .F. ) ;
#7951 = ORIENTED_EDGE ( 'NONE', *, *, #17583, .F. ) ;
#7952 = CARTESIAN_POINT ( 'NONE',  ( 137.2104978357160405, -3658.067685255075958, 2239.010000000090258 ) ) ;
#7953 = ORIENTED_EDGE ( 'NONE', *, *, #12214, .F. ) ;
#7954 = CARTESIAN_POINT ( 'NONE',  ( 145.1299181802738758, -3581.277546178230750, 2245.892459022343701 ) ) ;
#7956 = CIRCLE ( 'NONE', #14319, 3.606800000000021100 ) ;
#7955 = CALENDAR_DATE ( 2026, 26, 10 ) ;
#7957 = CARTESIAN_POINT ( 'NONE',  ( 145.4149999194000600, -3579.389963339004225, 2244.594906236255156 ) ) ;
#7958 = CARTESIAN_POINT ( 'NONE',  ( 25.39999999999999858, -3619.500000000000000, 2239.771999999999935 ) ) ;
#7959 = AXIS2_PLACEMENT_3D ( 'NONE', #13889, #8614, #10601 ) ;
#7960 = EDGE_CURVE ( 'NONE', #6861, #5300, #22200, .T. ) ;
#7961 = CARTESIAN_POINT ( 'NONE',  ( 15.54479972192533488, -3579.494999998566982, 2257.962943247991461 ) ) ;
#7962 = EDGE_CURVE ( 'NONE', #12400, #9540, #20315, .T. ) ;
#7963 = DIRECTION ( 'NONE',  ( 1.000000000000000000, 0.000000000000000000, 0.000000000000000000 ) ) ;
#7964 = AXIS2_PLACEMENT_3D ( 'NONE', #19778, #3705, #7462 ) ;
#7965 = DIRECTION ( 'NONE',  ( 0.000000000000000000, -1.000000000000000000, 0.000000000000000000 ) ) ;
#7966 = ORIENTED_EDGE ( 'NONE', *, *, #19119, .F. ) ;
#7967 = FACE_OUTER_BOUND ( 'NONE', #7563, .T. ) ;
#7968 = DIRECTION ( 'NONE',  ( 1.206643234470999950E-12, -1.000000000000000000, -2.336881798973999985E-14 ) ) ;
#7969 = ORIENTED_EDGE ( 'NONE', *, *, #12245, .F. ) ;
#7970 = FACE_OUTER_BOUND ( 'NONE', #2985, .T. ) ;
#7971 = CARTESIAN_POINT ( 'NONE',  ( 10.90366342691393164, -3657.299102526176739, 2247.222754898936728 ) ) ;
#7972 = CIRCLE ( 'NONE', #3463, 0.3809999999999993947 ) ;
#7973 = ORIENTED_EDGE ( 'NONE', *, *, #17102, .T. ) ;
#7974 = EDGE_LOOP ( 'NONE', ( #11051, #11857, #16273, #7790 ) ) ;
#7975 = ORIENTED_EDGE ( 'NONE', *, *, #2009, .F. ) ;
#7976 = DIRECTION ( 'NONE',  ( 0.000000000000000000, -1.000000000000000000, 0.000000000000000000 ) ) ;
#7977 = CIRCLE ( 'NONE', #10227, 5.079999999999973426 ) ;
#7978 = ORIENTED_EDGE ( 'NONE', *, *, #9825, .F. ) ;
#7979 = CIRCLE ( 'NONE', #4983, 0.7619999999999987894 ) ;
#7980 = FACE_OUTER_BOUND ( 'NONE', #15760, .T. ) ;
#7981 = CARTESIAN_POINT ( 'NONE',  ( 14.71696921254339685, -3577.486687656909453, 2249.884401328558397 ) ) ;
#7982 =( NAMED_UNIT ( * ) PLANE_ANGLE_UNIT ( ) SI_UNIT ( $, .RADIAN. ) );
#7983 = CARTESIAN_POINT ( 'NONE',  ( 142.0870141205355992, -3581.042503004332502, 2249.216714460935691 ) ) ;
#7984 = VERTEX_POINT ( 'NONE', #22312 ) ;
#7985 = CARTESIAN_POINT ( 'NONE',  ( 50.79999999999999716, -3670.300000000000182, 2261.869999999999891 ) ) ;
#7986 = SECURITY_CLASSIFICATION_LEVEL ( 'unclassified' ) ;
#7987 = CARTESIAN_POINT ( 'NONE',  ( 12.69999999999999929, -3653.027999999999793, 2263.117139999999836 ) ) ;
#7988 = DIRECTION ( 'NONE',  ( 1.000000000000000000, 0.000000000000000000, 0.000000000000000000 ) ) ;
#7989 = AXIS2_PLACEMENT_3D ( 'NONE', #2230, #7495, #11014 ) ;
#7990 = CARTESIAN_POINT ( 'NONE',  ( 134.2390000000000043, -3659.504999999999654, 2244.978999999999814 ) ) ;
#7991 = ORIENTED_EDGE ( 'NONE', *, *, #16735, .T. ) ;
#7992 = AXIS2_PLACEMENT_3D ( 'NONE', #5775, #487, #21593 ) ;
#7993 = CARTESIAN_POINT ( 'NONE',  ( 18.16100000000000136, -3659.504999999999654, 2244.978999999999814 ) ) ;
#7994 = EDGE_CURVE ( 'NONE', #19405, #12115, #3848, .T. ) ;
#7995 = CIRCLE ( 'NONE', #16945, 2.844799999998998796 ) ;
#7996 = ADVANCED_FACE ( 'NONE', ( #6168 ), #13304, .T. ) ;
#7997 = VERTEX_POINT ( 'NONE', #15299 ) ;
#7998 = EDGE_CURVE ( 'NONE', #22298, #10503, #19360, .T. ) ;
#7999 = VERTEX_POINT ( 'NONE', #13533 ) ;
#8000 =( BOUNDED_CURVE ( )  B_SPLINE_CURVE ( 3, ( #22943, #10182, #17327, #8441 ),
 .UNSPECIFIED., .F., .T. ) 
 B_SPLINE_CURVE_WITH_KNOTS ( ( 4, 4 ),
 ( 1.570796327224941002, 3.141592653589829531 ),
 .UNSPECIFIED. ) 
 CURVE ( )  GEOMETRIC_REPRESENTATION_ITEM ( )  RATIONAL_B_SPLINE_CURVE ( ( 1.000000000000000000, 0.8047378542257188627, 0.8047378542257188627, 1.000000000000000000 ) ) 
 REPRESENTATION_ITEM ( '' )  );
#8001 = CARTESIAN_POINT ( 'NONE',  ( 66.34479999999999222, -3594.099999999999909, 2261.869999999999891 ) ) ;
#8002 = ORIENTED_EDGE ( 'NONE', *, *, #6881, .T. ) ;
#8003 = DIRECTION ( 'NONE',  ( -2.903809793931999834E-13, 4.457650181899999573E-12, 1.000000000000000000 ) ) ;
#8004 = DIRECTION ( 'NONE',  ( 1.000000000000000000, 0.000000000000000000, -1.224646799147353207E-16 ) ) ;
#8005 = EDGE_CURVE ( 'NONE', #13997, #21361, #2716, .T. ) ;
#8006 = CIRCLE ( 'NONE', #18470, 0.7619999999999294005 ) ;
#8007 = ORIENTED_EDGE ( 'NONE', *, *, #11441, .F. ) ;
#8008 = CARTESIAN_POINT ( 'NONE',  ( 19.17699999999900129, -3599.497499999999945, 2295.829799999999977 ) ) ;
#8009 =( NAMED_UNIT ( * ) PLANE_ANGLE_UNIT ( ) SI_UNIT ( $, .RADIAN. ) );
#8010 = DIRECTION ( 'NONE',  ( -1.000000000000000000, 0.000000000000000000, 0.000000000000000000 ) ) ;
#8011 = CARTESIAN_POINT ( 'NONE',  ( 15.54479972192533488, -3579.494999998566982, 2257.962943247991461 ) ) ;
#8012 = EDGE_CURVE ( 'NONE', #6309, #2800, #18772, .T. ) ;
#8013 = APPLICATION_PROTOCOL_DEFINITION ( 'international standard', 'automotive_design', 2000, #4076 ) ;
#8014 = EDGE_CURVE ( 'NONE', #20229, #22764, #22553, .T. ) ;
#8015 = CARTESIAN_POINT ( 'NONE',  ( 0.000000000000000000, -3694.938000000000102, 2239.771999999999935 ) ) ;
#8016 = CARTESIAN_POINT ( 'NONE',  ( 63.50000000000000000, -3594.099999999999909, 2239.771999999999935 ) ) ;
#8017 = CARTESIAN_POINT ( 'NONE',  ( 59.89320000000000022, -3594.099999999999909, 2260.600000000000364 ) ) ;
#8018 = FACE_OUTER_BOUND ( 'NONE', #13151, .T. ) ;
#8019 = ORIENTED_EDGE ( 'NONE', *, *, #10984, .F. ) ;
#8020 = TOROIDAL_SURFACE ( 'NONE', #12502, 5.080000000000000071, 0.3810000000000000053 ) ;
#8021 = CARTESIAN_POINT ( 'NONE',  ( 136.9723221135144797, -3543.579977981522461, 2255.303759353553687 ) ) ;
#8022 = VECTOR ( 'NONE', #9220, 1000.000000000000227 ) ;
#8023 = ORIENTED_EDGE ( 'NONE', *, *, #5931, .F. ) ;
#8024 = PLANE ( 'NONE',  #9520 ) ;
#8025 = DIRECTION ( 'NONE',  ( 0.000000000000000000, 0.000000000000000000, 1.000000000000000000 ) ) ;
#8026 = VERTEX_POINT ( 'NONE', #21037 ) ;
#8027 = VERTEX_POINT ( 'NONE', #1693 ) ;
#8028 = DIRECTION ( 'NONE',  ( -0.6887494619146540265, 0.000000000000000000, -0.7249994335944508483 ) ) ;
#8029 = DIRECTION ( 'NONE',  ( 0.000000000000000000, 1.000000000000000000, 0.000000000000000000 ) ) ;
#8030 = CARTESIAN_POINT ( 'NONE',  ( 10.28172140950000113, -3601.007291280000118, 2279.551786969999739 ) ) ;
#8031 = LINE ( 'NONE', #868, #14573 ) ;
#8032 = CARTESIAN_POINT ( 'NONE',  ( 123.3932000000010021, -3619.500000000000000, 2260.600000000000364 ) ) ;
#8033 = AXIS2_PLACEMENT_3D ( 'NONE', #22787, #6763, #20932 ) ;
#8034 = DIRECTION ( 'NONE',  ( 0.000000000000000000, 0.000000000000000000, 1.000000000000000000 ) ) ;
#8035 = EDGE_LOOP ( 'NONE', ( #20051, #3522, #5640, #21614 ) ) ;
#8036 = PERSON_AND_ORGANIZATION_ROLE ( 'creator' ) ;
#8037 = CIRCLE ( 'NONE', #4292, 5.460999999999938126 ) ;
#8038 = AXIS2_PLACEMENT_3D ( 'NONE', #1568, #13644, #8375 ) ;
#8039 = CARTESIAN_POINT ( 'NONE',  ( 145.1018191042290084, -3657.638755556700744, 2246.035947349423623 ) ) ;
#8040 = CARTESIAN_POINT ( 'NONE',  ( 9.862268097132236733, -3579.717233113928614, 2250.106397596277475 ) ) ;
#8041 = CARTESIAN_POINT ( 'NONE',  ( 57.14999999999999858, -3544.570000000000164, 2247.392000000000280 ) ) ;
#8042 = ORIENTED_EDGE ( 'NONE', *, *, #7568, .F. ) ;
#8043 = CARTESIAN_POINT ( 'NONE',  ( 28.24479999999899604, -3619.500000000000000, 2239.771999999999935 ) ) ;
#8044 = TOROIDAL_SURFACE ( 'NONE', #20036, 4.114799999999999791, 1.270000000000000018 ) ;
#8045 = CARTESIAN_POINT ( 'NONE',  ( 64.76999999999999602, -3544.061999999999898, 2289.213099999999940 ) ) ;
#8046 = CARTESIAN_POINT ( 'NONE',  ( 145.1961821871802272, -3661.071248187899528, 2244.703885868029829 ) ) ;
#8047 = EDGE_LOOP ( 'NONE', ( #506, #5063, #2283, #5490, #2234 ) ) ;
#8048 = DIRECTION ( 'NONE',  ( 3.410944169536999938E-12, -1.000000000000000000, -9.896505939572001285E-13 ) ) ;
#8049 = AXIS2_PLACEMENT_3D ( 'NONE', #3406, #10559, #11358 ) ;
#8050 = CARTESIAN_POINT ( 'NONE',  ( 14.79088965948426804, -3661.435447629304235, 2249.925490890767378 ) ) ;
#8051 = APPROVAL ( #3044, 'UNSPECIFIED' ) ;
#8052 = AXIS2_PLACEMENT_3D ( 'NONE', #22937, #7037, #19441 ) ;
#8053 = CARTESIAN_POINT ( 'NONE',  ( 12.69999999999999929, -3599.497499999999945, 2290.622800000000097 ) ) ;
#8054 = AXIS2_PLACEMENT_3D ( 'NONE', #5649, #10912, #9041 ) ;
#8055 = ORIENTED_EDGE ( 'NONE', *, *, #18163, .F. ) ;
#8056 = PLANE ( 'NONE',  #5457 ) ;
#8057 = DIRECTION ( 'NONE',  ( -1.000000000000000000, 0.000000000000000000, 0.000000000000000000 ) ) ;
#8058 = EDGE_CURVE ( 'NONE', #928, #21153, #10367, .T. ) ;
#8059 = DIRECTION ( 'NONE',  ( 0.000000000000000000, 0.000000000000000000, -1.000000000000000000 ) ) ;
#8060 = CARTESIAN_POINT ( 'NONE',  ( 15.48600340796466135, -3658.926920653574598, 2249.965218490672214 ) ) ;
#8061 = FACE_OUTER_BOUND ( 'NONE', #236, .T. ) ;
#8062 = VERTEX_POINT ( 'NONE', #4859 ) ;
#8063 = ORIENTED_EDGE ( 'NONE', *, *, #20537, .T. ) ;
#8064 = EDGE_CURVE ( 'NONE', #3958, #19453, #937, .T. ) ;
#8065 = FACE_OUTER_BOUND ( 'NONE', #11000, .T. ) ;
#8066 = VERTEX_POINT ( 'NONE', #19507 ) ;
#8067 = VERTEX_POINT ( 'NONE', #10247 ) ;
#8068 = CARTESIAN_POINT ( 'NONE',  ( 145.1457547493498055, -3581.228764793822393, 2245.816281768045428 ) ) ;
#8069 = AXIS2_PLACEMENT_3D ( 'NONE', #4793, #8080, #11472 ) ;
#8070 = CONTEXT_DEPENDENT_SHAPE_REPRESENTATION ( #221, #20257 ) ;
#8071 = TOROIDAL_SURFACE ( 'NONE', #4702, 3.606799999999999784, 0.7620000000000000107 ) ;
#8072 = CARTESIAN_POINT ( 'NONE',  ( 139.6999999999999886, -3576.650200000000950, 2257.592639999999847 ) ) ;
#8073 = CARTESIAN_POINT ( 'NONE',  ( 17.77895441395078890, -3662.125108044190711, 2245.354081002604289 ) ) ;
#8074 = CARTESIAN_POINT ( 'NONE',  ( 12.79208108087000006, -3656.660200000000259, 2257.592639999999847 ) ) ;
#8075 = FACE_OUTER_BOUND ( 'NONE', #6006, .T. ) ;
#8076 = VECTOR ( 'NONE', #17251, 1000.000000000000000 ) ;
#8077 = DIRECTION ( 'NONE',  ( -0.8660254037840939834, -0.5000000000005969669, 0.000000000000000000 ) ) ;
#8078 = ORIENTED_EDGE ( 'NONE', *, *, #16885, .T. ) ;
#8079 = DIRECTION ( 'NONE',  ( 1.224646799141920914E-16, -1.000000000000000000, -2.336881798971000421E-14 ) ) ;
#8080 = DIRECTION ( 'NONE',  ( 0.000000000000000000, 1.000000000000000000, 0.000000000000000000 ) ) ;
#8081 = EDGE_LOOP ( 'NONE', ( #5764, #22807, #8611, #21806, #20785, #35 ) ) ;
#8082 = CIRCLE ( 'NONE', #21915, 2.844800000000001550 ) ;
#8084 = DIRECTION ( 'NONE',  ( 1.000000000000000000, 0.000000000000000000, 1.344534956950000190E-13 ) ) ;
#8083 = B_SPLINE_CURVE_WITH_KNOTS ( 'NONE', 3,
 ( #21551, #227, #5507, #12642, #3722, #10880, #1979, #9128, #16271, #5618, #12870, #3844, #10995, #18137, #2101, #9243, #334 ),
 .UNSPECIFIED., .F., .F.,
 ( 4, 1, 1, 1, 1, 1, 1, 1, 1, 1, 1, 1, 1, 1, 4 ),
 ( 0.000000000000000000, 0.07142857142856999519, 0.1428571428570999946, 0.2142857142857000075, 0.2857142857143000203, 0.3571428571429000054, 0.4285714285713999594, 0.5000000000000000000, 0.5714285714286000406, 0.6428571428570999391, 0.7142857142856999797, 0.7857142857142999093, 0.8571428571429000609, 0.9285714285714000704, 1.000000000000000000 ),
 .UNSPECIFIED. ) ;
#8085 = CARTESIAN_POINT ( 'NONE',  ( 142.5447999999989861, -3659.504999999999654, 2257.962944264955695 ) ) ;
#8086 = CIRCLE ( 'NONE', #14818, 3.175000000000149925 ) ;
#8087 = VERTEX_POINT ( 'NONE', #1341 ) ;
#8088 = AXIS2_PLACEMENT_3D ( 'NONE', #23049, #16260, #21656 ) ;
#8089 = ORIENTED_EDGE ( 'NONE', *, *, #2929, .F. ) ;
#8090 = EDGE_CURVE ( 'NONE', #2972, #9357, #8721, .T. ) ;
#8091 = VERTEX_POINT ( 'NONE', #3329 ) ;
#8092 = PERSON_AND_ORGANIZATION_ROLE ( 'classification_officer' ) ;
#8093 = DIRECTION ( 'NONE',  ( 0.000000000000000000, 0.000000000000000000, 1.000000000000000000 ) ) ;
#8094 = CIRCLE ( 'NONE', #12961, 2.844800000000091700 ) ;
#8095 = EDGE_CURVE ( 'NONE', #18734, #7197, #11695, .T. ) ;
#8096 = ORIENTED_EDGE ( 'NONE', *, *, #1029, .F. ) ;
#8097 = ADVANCED_FACE ( 'NONE', ( #10480 ), #1575, .T. ) ;
#8098 = LINE ( 'NONE', #8205, #17099 ) ;
#8099 = CARTESIAN_POINT ( 'NONE',  ( 10.97145801871307924, -3577.235475337109165, 2249.727398826565604 ) ) ;
#8100 = DIRECTION ( 'NONE',  ( 1.000000000000000000, 0.000000000000000000, 0.000000000000000000 ) ) ;
#8101 = CIRCLE ( 'NONE', #11093, 2.844800000000091700 ) ;
#8102 = CIRCLE ( 'NONE', #16329, 2.844799999999994444 ) ;
#8103 = DIRECTION ( 'NONE',  ( 0.000000000000000000, -1.000000000000000000, 0.000000000000000000 ) ) ;
#8104 = VERTEX_POINT ( 'NONE', #20921 ) ;
#8105 = CARTESIAN_POINT ( 'NONE',  ( 136.8552000000009912, -3659.693686221675307, 2257.962944264956150 ) ) ;
#8106 = APPROVAL_DATE_TIME ( #20511, #2891 ) ;
#8107 = CARTESIAN_POINT ( 'NONE',  ( -12.69999999999999929, -3578.860000000000127, 2247.392000000000280 ) ) ;
#8108 = FACE_OUTER_BOUND ( 'NONE', #9184, .T. ) ;
#8109 = PRODUCT_DEFINITION_SHAPE ( 'NONE', 'NONE',  #15652 ) ;
#8110 = VECTOR ( 'NONE', #7203, 1000.000000000000000 ) ;
#8111 = ADVANCED_FACE ( 'NONE', ( #13891 ), #17382, .T. ) ;
#8112 = VERTEX_POINT ( 'NONE', #7095 ) ;
#8113 = AXIS2_PLACEMENT_3D ( 'NONE', #14595, #18217, #638 ) ;
#8114 = VECTOR ( 'NONE', #2855, 1000.000000000000000 ) ;
#8115 = CARTESIAN_POINT ( 'NONE',  ( 142.2944679814244751, -3660.711379646646492, 2250.192293398927632 ) ) ;
#8116 = ORIENTED_EDGE ( 'NONE', *, *, #13590, .F. ) ;
#8117 = ORIENTED_EDGE ( 'NONE', *, *, #4263, .T. ) ;
#8118 = CARTESIAN_POINT ( 'NONE',  ( 10.16000000000000014, -3544.570000000000164, 2255.774000000000342 ) ) ;
#8119 = ORIENTED_EDGE ( 'NONE', *, *, #11851, .F. ) ;
#8120 = DIRECTION ( 'NONE',  ( 1.000000000000000000, 0.000000000000000000, 1.165588477298000095E-13 ) ) ;
#8121 = DIRECTION ( 'NONE',  ( -1.000000000000000000, 0.000000000000000000, 0.000000000000000000 ) ) ;
#8122 = AXIS2_PLACEMENT_3D ( 'NONE', #9964, #22152, #7873 ) ;
#8123 = EDGE_LOOP ( 'NONE', ( #20577, #23111 ) ) ;
#8124 = EDGE_CURVE ( 'NONE', #22852, #11037, #19699, .T. ) ;
#8125 = AXIS2_PLACEMENT_3D ( 'NONE', #15155, #22282, #12217 ) ;
#8126 = DIRECTION ( 'NONE',  ( 0.000000000000000000, 0.000000000000000000, -1.000000000000000000 ) ) ;
#8127 = DIRECTION ( 'NONE',  ( 0.000000000000000000, -1.000000000000000000, 0.000000000000000000 ) ) ;
#8128 = FACE_OUTER_BOUND ( 'NONE', #17910, .T. ) ;
#8129 = APPROVAL_STATUS ( 'not_yet_approved' ) ;
#8130 = ADVANCED_FACE ( 'NONE', ( #8505 ), #11822, .T. ) ;
#8131 = EDGE_CURVE ( 'NONE', #19682, #4249, #14830, .T. ) ;
#8132 = DIRECTION ( 'NONE',  ( -0.6887494619147132013, 0.000000000000000000, 0.7249994335943947821 ) ) ;
#8133 = DIRECTION ( 'NONE',  ( 1.000000000000000000, 0.000000000000000000, 0.000000000000000000 ) ) ;
#8134 = DIRECTION ( 'NONE',  ( -1.000000000000000000, 0.000000000000000000, 0.000000000000000000 ) ) ;
#8135 = DIRECTION ( 'NONE',  ( 1.000000000000000000, 0.000000000000000000, 0.000000000000000000 ) ) ;
#8136 = EDGE_CURVE ( 'NONE', #21944, #15061, #19279, .T. ) ;
#8137 = ORIENTED_EDGE ( 'NONE', *, *, #11146, .F. ) ;
#8138 =( BOUNDED_CURVE ( )  B_SPLINE_CURVE ( 3, ( #2018, #14563, #2249, #9402 ),
 .UNSPECIFIED., .F., .F. ) 
 B_SPLINE_CURVE_WITH_KNOTS ( ( 4, 4 ),
 ( -9.769962616701377556E-15, 1.570796327117804925 ),
 .UNSPECIFIED. ) 
 CURVE ( )  GEOMETRIC_REPRESENTATION_ITEM ( )  RATIONAL_B_SPLINE_CURVE ( ( 1.000000000000000000, 0.8047378540482524878, 0.8047378540482524878, 1.000000000000000000 ) ) 
 REPRESENTATION_ITEM ( '' )  );
#8139 = CARTESIAN_POINT ( 'NONE',  ( 137.1349247998588794, -3544.173420539443214, 2255.711168198842643 ) ) ;
#8140 = AXIS2_PLACEMENT_3D ( 'NONE', #9260, #119, #12651 ) ;
#8141 = ORIENTED_EDGE ( 'NONE', *, *, #9235, .T. ) ;
#8142 = ADVANCED_FACE ( 'NONE', ( #22777 ), #8850, .T. ) ;
#8143 = DIRECTION ( 'NONE',  ( 0.000000000000000000, 0.000000000000000000, 1.000000000000000000 ) ) ;
#8144 = ADVANCED_FACE ( 'NONE', ( #1221 ), #6638, .T. ) ;
#8145 = AXIS2_PLACEMENT_3D ( 'NONE', #1057, #13838, #3162 ) ;
#8146 = ORIENTED_EDGE ( 'NONE', *, *, #18717, .T. ) ;
#8147 = ORIENTED_EDGE ( 'NONE', *, *, #18262, .T. ) ;
#8148 = CARTESIAN_POINT ( 'NONE',  ( 63.50000000000000000, -3644.899999999999636, 2260.600000000000364 ) ) ;
#8149 = CARTESIAN_POINT ( 'NONE',  ( -12.31900000000000084, -3578.860000000000127, 2247.392000000000280 ) ) ;
#8150 = CYLINDRICAL_SURFACE ( 'NONE', #6975, 2.844799999999999773 ) ;
#8151 = CYLINDRICAL_SURFACE ( 'NONE', #7109, 0.7619999999999294005 ) ;
#8152 = DIRECTION ( 'NONE',  ( -3.592637833098024570E-12, 0.5000000000004030110, -0.8660254037842058938 ) ) ;
#8153 = CARTESIAN_POINT ( 'NONE',  ( 21.79320000000099711, -3568.700000000000273, 2259.837999999999738 ) ) ;
#8154 = DIRECTION ( 'NONE',  ( 0.000000000000000000, 0.000000000000000000, -1.000000000000000000 ) ) ;
#8155 = VERTEX_POINT ( 'NONE', #13778 ) ;
#8156 = APPROVAL_DATE_TIME ( #10133, #5791 ) ;
#8157 = CIRCLE ( 'NONE', #2176, 1.269999999999882334 ) ;
#8158 = EDGE_CURVE ( 'NONE', #22556, #15415, #19161, .T. ) ;
#8159 = EDGE_LOOP ( 'NONE', ( #2035, #9298, #8042, #9055 ) ) ;
#8160 = CARTESIAN_POINT ( 'NONE',  ( 145.3865858764642383, -3658.926257878062643, 2244.815985133692266 ) ) ;
#8161 = AXIS2_PLACEMENT_3D ( 'NONE', #7666, #21959, #407 ) ;
#8162 = DIRECTION ( 'NONE',  ( 1.000000000000000000, 0.000000000000000000, 0.000000000000000000 ) ) ;
#8163 = LINE ( 'NONE', #6297, #7833 ) ;
#8164 = ORIENTED_EDGE ( 'NONE', *, *, #10057, .T. ) ;
#8165 = CARTESIAN_POINT ( 'NONE',  ( 12.69999999999999929, -3583.940000000000055, 2268.705139999999574 ) ) ;
#8166 = CARTESIAN_POINT ( 'NONE',  ( 145.3787012162004544, -3660.148468257834793, 2244.547209130087140 ) ) ;
#8167 = EDGE_LOOP ( 'NONE', ( #3089, #22710, #38, #685 ) ) ;
#8168 = CARTESIAN_POINT ( 'NONE',  ( 12.69999999997562057, -3602.189900000083526, 2296.210799999999836 ) ) ;
#8169 = EDGE_CURVE ( 'NONE', #3614, #10242, #19993, .T. ) ;
#8170 = CARTESIAN_POINT ( 'NONE',  ( 14.73423477643819268, -3661.495730106304563, 2249.893851560407256 ) ) ;
#8171 = AXIS2_PLACEMENT_3D ( 'NONE', #6813, #5049, #22732 ) ;
#8172 = CARTESIAN_POINT ( 'NONE',  ( 12.69999999999999929, -3649.471999999999753, 2268.705139999999574 ) ) ;
#8173 = ORIENTED_EDGE ( 'NONE', *, *, #4070, .T. ) ;
#8174 = CARTESIAN_POINT ( 'NONE',  ( 7.387125747139000609, -3581.600847139000052, 2246.630000000000109 ) ) ;
#8175 = CARTESIAN_POINT ( 'NONE',  ( 142.0316867971999955, -3660.851200000000063, 2242.820000000000164 ) ) ;
#8176 = CARTESIAN_POINT ( 'NONE',  ( 142.7470794804999912, -3695.699999999999818, 2254.503999999999905 ) ) ;
#8177 = DIRECTION ( 'NONE',  ( 0.000000000000000000, -1.000000000000000000, 0.000000000000000000 ) ) ;
#8178 = EDGE_LOOP ( 'NONE', ( #1226, #2847 ) ) ;
#8179 = ORIENTED_EDGE ( 'NONE', *, *, #4576, .T. ) ;
#8180 = DIRECTION ( 'NONE',  ( -1.000000000000000000, 0.000000000000000000, 0.000000000000000000 ) ) ;
#8181 = EDGE_LOOP ( 'NONE', ( #12059, #17886, #12343, #5615, #15936 ) ) ;
#8182 = DIRECTION ( 'NONE',  ( 2.008939161382000013E-12, 1.000000000000000000, 3.793660610075000646E-12 ) ) ;
#8183 = CALENDAR_DATE ( 2026, 26, 10 ) ;
#8184 = APPLIED_PERSON_AND_ORGANIZATION_ASSIGNMENT ( #18716, #16961, ( #16481 ) ) ;
#8185 = CARTESIAN_POINT ( 'NONE',  ( 35.56000000000000227, -3543.299999999999727, 2247.392000000000280 ) ) ;
#8186 = CARTESIAN_POINT ( 'NONE',  ( 12.69999999999999929, -3659.504999999999654, 2245.359999999999673 ) ) ;
#8187 = CARTESIAN_POINT ( 'NONE',  ( 17.58955766687454769, -3662.463685539857579, 2245.750755658854814 ) ) ;
#8188 = CIRCLE ( 'NONE', #22762, 0.7619999999999294005 ) ;
#8189 = CARTESIAN_POINT ( 'NONE',  ( 15.44319999999931525, -3660.383257047475126, 2255.967040000000907 ) ) ;
#8190 = CARTESIAN_POINT ( 'NONE',  ( 124.1552000000010025, -3619.500000000000000, 2259.837999999999738 ) ) ;
#8191 = B_SPLINE_CURVE_WITH_KNOTS ( 'NONE', 3,
 ( #14035, #21187, #10275, #15439 ),
 .UNSPECIFIED., .F., .F.,
 ( 4, 4 ),
 ( 0.000000000000000000, 1.000000000000000000 ),
 .UNSPECIFIED. ) ;
#8192 = CARTESIAN_POINT ( 'NONE',  ( 11.34365660141000021, -3637.153244320999875, 2296.210799999999836 ) ) ;
#8193 = EDGE_LOOP ( 'NONE', ( #11048, #8096, #18351, #20030 ) ) ;
#8194 = DIRECTION ( 'NONE',  ( -1.000000000000000000, 0.000000000000000000, 0.000000000000000000 ) ) ;
#8195 = CYLINDRICAL_SURFACE ( 'NONE', #575, 11.11249999999985860 ) ;
#8196 = ORIENTED_EDGE ( 'NONE', *, *, #516, .T. ) ;
#8197 = PLANE ( 'NONE',  #2807 ) ;
#8198 = CARTESIAN_POINT ( 'NONE',  ( 10.63228947054044760, -3657.550950343449131, 2248.571178883313223 ) ) ;
#8199 = VERTEX_POINT ( 'NONE', #13055 ) ;
#8200 = EDGE_LOOP ( 'NONE', ( #4823, #14261, #12308, #2799 ) ) ;
#8201 = VERTEX_POINT ( 'NONE', #14587 ) ;
#8202 = DIRECTION ( 'NONE',  ( -1.286674632898999957E-12, -1.000000000000000000, 0.000000000000000000 ) ) ;
#8203 = AXIS2_PLACEMENT_3D ( 'NONE', #4503, #10365, #11642 ) ;
#8204 = ORIENTED_EDGE ( 'NONE', *, *, #7385, .F. ) ;
#8205 = CARTESIAN_POINT ( 'NONE',  ( -12.31900000000000084, -3577.513800000000174, 2245.060313203000078 ) ) ;
#8206 = FACE_OUTER_BOUND ( 'NONE', #18450, .T. ) ;
#8207 = CARTESIAN_POINT ( 'NONE',  ( 0.000000000000000000, 0.000000000000000000, 0.000000000000000000 ) ) ;
#8208 = CARTESIAN_POINT ( 'NONE',  ( 142.2925313698394234, -3580.666266504254054, 2249.589929609103820 ) ) ;
#8209 = ORIENTED_EDGE ( 'NONE', *, *, #12730, .F. ) ;
#8210 = CARTESIAN_POINT ( 'NONE',  ( 137.8183059914243245, -3581.636540092137693, 2257.752309752018391 ) ) ;
#8211 = CALENDAR_DATE ( 2026, 26, 10 ) ;
#8212 = APPLIED_PERSON_AND_ORGANIZATION_ASSIGNMENT ( #10804, #22982, ( #12377 ) ) ;
#8213 = EDGE_CURVE ( 'NONE', #2120, #565, #5780, .T. ) ;
#8214 = CARTESIAN_POINT ( 'NONE',  ( 15.41268679701111566, -3637.936329547520472, 2296.591799999999694 ) ) ;
#8215 = AXIS2_PLACEMENT_3D ( 'NONE', #21285, #19403, #4991 ) ;
#8216 = CARTESIAN_POINT ( 'NONE',  ( 134.2764082060851933, -3657.703343431524900, 2245.923799496059928 ) ) ;
#8217 = ADVANCED_FACE ( 'NONE', ( #7439 ), #8764, .T. ) ;
#8218 = ADVANCED_FACE ( 'NONE', ( #3915 ), #21846, .T. ) ;
#8219 = ORIENTED_EDGE ( 'NONE', *, *, #829, .T. ) ;
#8220 = CARTESIAN_POINT ( 'NONE',  ( 142.1265142685761873, -3660.990011674679408, 2250.106896142239293 ) ) ;
#8221 = EDGE_CURVE ( 'NONE', #4633, #6290, #20880, .T. ) ;
#8222 = ORIENTED_EDGE ( 'NONE', *, *, #7421, .T. ) ;
#8223 = CARTESIAN_POINT ( 'NONE',  ( 12.69999999999999929, -3649.471999999999753, 2268.705139999999574 ) ) ;
#8224 = LINE ( 'NONE', #22851, #5056 ) ;
#8225 = ORIENTED_EDGE ( 'NONE', *, *, #501, .T. ) ;
#8226 = EDGE_CURVE ( 'NONE', #13348, #21213, #17869, .T. ) ;
#8227 = VERTEX_POINT ( 'NONE', #5688 ) ;
#8228 = CARTESIAN_POINT ( 'NONE',  ( 136.9873132028999976, -3661.071170452999922, 2239.009999999999764 ) ) ;
#8229 = FACE_OUTER_BOUND ( 'NONE', #4682, .T. ) ;
#8230 = AXIS2_PLACEMENT_3D ( 'NONE', #14193, #1760, #7155 ) ;
#8231 = ORIENTED_EDGE ( 'NONE', *, *, #1926, .F. ) ;
#8232 = CARTESIAN_POINT ( 'NONE',  ( -5.588000000000000078, -3660.140000000000327, 2250.998800000000301 ) ) ;
#8233 = DIRECTION ( 'NONE',  ( -1.000000000000000000, 0.000000000000000000, 0.000000000000000000 ) ) ;
#8234 = APPLIED_APPROVAL_ASSIGNMENT ( #18651, ( #381 ) ) ;
#8235 = EDGE_CURVE ( 'NONE', #20799, #13309, #9080, .T. ) ;
#8236 = LINE ( 'NONE', #9532, #11471 ) ;
#8237 = DATE_AND_TIME ( #12099, #20204 ) ;
#8238 = EDGE_CURVE ( 'NONE', #5100, #12459, #1372, .T. ) ;
#8239 = CARTESIAN_POINT ( 'NONE',  ( 1.270000000000000018, -3695.699999999999818, 2259.329999999999927 ) ) ;
#8240 = CARTESIAN_POINT ( 'NONE',  ( 139.6999999999999886, -3659.504999999999654, 2244.978999999999814 ) ) ;
#8241 = DIRECTION ( 'NONE',  ( 0.000000000000000000, 0.000000000000000000, 1.000000000000000000 ) ) ;
#8242 = CARTESIAN_POINT ( 'NONE',  ( 141.8175935050403780, -3657.605346374574765, 2248.683677737056314 ) ) ;
#8243 = FACE_OUTER_BOUND ( 'NONE', #10536, .T. ) ;
#8244 = ORIENTED_EDGE ( 'NONE', *, *, #10684, .T. ) ;
#8245 = DIRECTION ( 'NONE',  ( -1.648694042066000049E-12, -1.000000000000000000, 0.000000000000000000 ) ) ;
#8246 = CIRCLE ( 'NONE', #8620, 3.175000000000149925 ) ;
#8247 = ADVANCED_FACE ( 'NONE', ( #14703 ), #9983, .T. ) ;
#8248 = PRODUCT_DEFINITION_FORMATION_WITH_SPECIFIED_SOURCE ( 'ANY', '', #785, .NOT_KNOWN. ) ;
#8249 = APPLIED_APPROVAL_ASSIGNMENT ( #16097, ( #16119 ) ) ;
#8250 = ORIENTED_EDGE ( 'NONE', *, *, #9513, .F. ) ;
#8251 = DIRECTION ( 'NONE',  ( 0.000000000000000000, 0.000000000000000000, -1.000000000000000000 ) ) ;
#8252 = ADVANCED_FACE ( 'NONE', ( #16564 ), #20833, .T. ) ;
#8253 = EDGE_CURVE ( 'NONE', #6304, #18734, #10720, .T. ) ;
#8254 = CARTESIAN_POINT ( 'NONE',  ( -0.7620000000000000107, -3578.860000000000127, 2247.392000000000280 ) ) ;
#8255 = EDGE_LOOP ( 'NONE', ( #14736, #21117, #2275, #15215 ) ) ;
#8256 = VERTEX_POINT ( 'NONE', #174 ) ;
#8257 = DIRECTION ( 'NONE',  ( 0.000000000000000000, 0.000000000000000000, -1.000000000000000000 ) ) ;
#8258 = CARTESIAN_POINT ( 'NONE',  ( 3.048000000000000043, -3694.938000000000102, 2228.849999999999909 ) ) ;
#8259 = DIRECTION ( 'NONE',  ( -1.000000000000000000, 0.000000000000000000, 0.000000000000000000 ) ) ;
#8260 = VERTEX_POINT ( 'NONE', #16112 ) ;
#8261 = DIRECTION ( 'NONE',  ( 1.000000000000000000, 0.000000000000000000, 0.000000000000000000 ) ) ;
#8262 = LINE ( 'NONE', #15067, #9465 ) ;
#8263 = EDGE_CURVE ( 'NONE', #5209, #1371, #5920, .T. ) ;
#8264 = CARTESIAN_POINT ( 'NONE',  ( 18.13822863179804301, -3577.698793233671040, 2244.777281343887807 ) ) ;
#8265 = CARTESIAN_POINT ( 'NONE',  ( 0.000000000000000000, -3544.570000000000164, 2259.329999999999927 ) ) ;
#8266 = EDGE_LOOP ( 'NONE', ( #18650, #7238, #2053, #19593, #9281, #10042 ) ) ;
#8267 = DATE_AND_TIME ( #15301, #20235 ) ;
#8268 = EDGE_LOOP ( 'NONE', ( #2793, #17368 ) ) ;
#8269 = CARTESIAN_POINT ( 'NONE',  ( 47.19319999999999737, -3619.500000000000000, 2239.009999999999764 ) ) ;
#8270 = LOCAL_TIME ( 17, 37, 43.00000000000000000, #1964 ) ;
#8271 = APPLIED_APPROVAL_ASSIGNMENT ( #5791, ( #6775 ) ) ;
#8272 = CARTESIAN_POINT ( 'NONE',  ( 10.41817338763723022, -3581.193830325411454, 2249.018787504950069 ) ) ;
#8273 = DIRECTION ( 'NONE',  ( 0.000000000000000000, -1.000000000000000000, 0.000000000000000000 ) ) ;
#8274 = ORIENTED_EDGE ( 'NONE', *, *, #5543, .T. ) ;
#8275 = CARTESIAN_POINT ( 'NONE',  ( 12.70000000002640839, -3576.802599999929498, 2239.391000000000076 ) ) ;
#8276 = CIRCLE ( 'NONE', #6782, 5.460999999999938126 ) ;
#8277 = CARTESIAN_POINT ( 'NONE',  ( 144.8225857063939372, -3662.039185438572531, 2245.272442455612236 ) ) ;
#8278 = CARTESIAN_POINT ( 'NONE',  ( 15.44319999999931525, -3578.616742952524419, 2255.967040000000907 ) ) ;
#8279 = DIRECTION ( 'NONE',  ( 0.000000000000000000, 0.000000000000000000, 1.000000000000000000 ) ) ;
#8280 = ADVANCED_FACE ( 'NONE', ( #7206 ), #15228, .T. ) ;
#8281 = ADVANCED_FACE ( 'NONE', ( #14359 ), #12600, .F. ) ;
#8282 = CARTESIAN_POINT ( 'NONE',  ( 139.6999999999999886, -3579.494999999999891, 2270.760000000000218 ) ) ;
#8283 = ORIENTED_EDGE ( 'NONE', *, *, #19549, .F. ) ;
#8284 = ADVANCED_FACE ( 'NONE', ( #5575 ), #19861, .F. ) ;
#8285 = APPLIED_APPROVAL_ASSIGNMENT ( #17193, ( #2304 ) ) ;
#8286 = DIRECTION ( 'NONE',  ( 0.000000000000000000, -1.000000000000000000, 0.000000000000000000 ) ) ;
#8287 = CARTESIAN_POINT ( 'NONE',  ( 15.54479999999999862, -3639.397331916999974, 2279.447335734999797 ) ) ;
#8288 = DIRECTION ( 'NONE',  ( 1.000000000000000000, 0.000000000000000000, 0.000000000000000000 ) ) ;
#8289 = DIRECTION ( 'NONE',  ( -0.000000000000000000, -1.000000000000000000, -0.000000000000000000 ) ) ;
#8290 = CARTESIAN_POINT ( 'NONE',  ( 20.62424768829000143, -3694.430000000000291, 2260.600000000000364 ) ) ;
#8291 = ORIENTED_EDGE ( 'NONE', *, *, #3254, .T. ) ;
#8292 = ADVANCED_FACE ( 'NONE', ( #8128 ), #9868, .F. ) ;
#8293 = VECTOR ( 'NONE', #1347, 1000.000000000000000 ) ;
#8294 = EDGE_LOOP ( 'NONE', ( #802, #11257, #21638, #7595 ) ) ;
#8295 = AXIS2_PLACEMENT_3D ( 'NONE', #21352, #2950, #2012 ) ;
#8296 = CARTESIAN_POINT ( 'NONE',  ( 10.36831320282916380, -3600.843700000149056, 2296.433984632680676 ) ) ;
#8297 = ORIENTED_EDGE ( 'NONE', *, *, #14853, .T. ) ;
#8298 = B_SPLINE_CURVE_WITH_KNOTS ( 'NONE', 3,
 ( #11643, #16922, #18579, #15412 ),
 .UNSPECIFIED., .F., .F.,
 ( 4, 4 ),
 ( 0.000000000000000000, 1.000000000000000000 ),
 .UNSPECIFIED. ) ;
#8299 = CARTESIAN_POINT ( 'NONE',  ( 9.787381488757823433, -3543.344914975609754, 2254.841485305899823 ) ) ;
#8300 = CONTEXT_DEPENDENT_SHAPE_REPRESENTATION ( #22499, #11083 ) ;
#8301 = EDGE_CURVE ( 'NONE', #8104, #3611, #22695, .T. ) ;
#8302 = CYLINDRICAL_SURFACE ( 'NONE', #2696, 2.844799999999009010 ) ;
#8303 = EDGE_CURVE ( 'NONE', #6172, #23061, #6372, .T. ) ;
#8304 = CYLINDRICAL_SURFACE ( 'NONE', #16834, 2.844800000000091700 ) ;
#8305 = CARTESIAN_POINT ( 'NONE',  ( 11.61844525849999954, -3662.141125287999785, 2257.644379465999918 ) ) ;
#8306 = CARTESIAN_POINT ( 'NONE',  ( 15.54479999999932716, -3659.956214629474744, 2256.063560000000962 ) ) ;
#8307 = DIRECTION ( 'NONE',  ( 1.000000000000000000, 0.000000000000000000, 0.000000000000000000 ) ) ;
#8308 = FACE_OUTER_BOUND ( 'NONE', #17054, .T. ) ;
#8309 = ORIENTED_EDGE ( 'NONE', *, *, #10357, .F. ) ;
#8310 = AXIS2_PLACEMENT_3D ( 'NONE', #3190, #9870, #4723 ) ;
#8311 = CARTESIAN_POINT ( 'NONE',  ( 101.5999999999999943, -3568.700000000000273, 2260.600000000000364 ) ) ;
#8312 = TOROIDAL_SURFACE ( 'NONE', #18413, 5.080000000000000071, 0.3810000000000000053 ) ;
#8313 = LINE ( 'NONE', #8432, #13297 ) ;
#8314 = ORIENTED_EDGE ( 'NONE', *, *, #12013, .F. ) ;
#8315 = CARTESIAN_POINT ( 'NONE',  ( 134.6199999999999761, -3579.494999999999891, 2245.359999999999673 ) ) ;
#8316 = CARTESIAN_POINT ( 'NONE',  ( 139.6999999999999886, -3579.494999999999891, 2255.774000000000342 ) ) ;
#8317 = ORIENTED_EDGE ( 'NONE', *, *, #21324, .T. ) ;
#8318 = EDGE_LOOP ( 'NONE', ( #8799, #6548, #20434, #8603 ) ) ;
#8319 = CARTESIAN_POINT ( 'NONE',  ( 134.0487369367239694, -3580.386377785477634, 2244.978268890278741 ) ) ;
#8320 = PRODUCT_DEFINITION_CONTEXT ( 'detailed design', #6476, 'design' ) ;
#8321 = AXIS2_PLACEMENT_3D ( 'NONE', #13082, #11775, #998 ) ;
#8322 = ORIENTED_EDGE ( 'NONE', *, *, #12974, .F. ) ;
#8323 = DIRECTION ( 'NONE',  ( -1.000000000000000000, 0.000000000000000000, 0.000000000000000000 ) ) ;
#8324 = DIRECTION ( 'NONE',  ( 1.000000000000000000, 0.000000000000000000, 0.000000000000000000 ) ) ;
#8325 = DIRECTION ( 'NONE',  ( 1.000000000000000000, 0.000000000000000000, 0.000000000000000000 ) ) ;
#8326 = CARTESIAN_POINT ( 'NONE',  ( 136.9738742589587162, -3580.309117874636740, 2249.840541574770668 ) ) ;
#8327 = TOROIDAL_SURFACE ( 'NONE', #4209, 5.080000000000000071, 0.3810000000000000053 ) ;
#8328 = ORIENTED_EDGE ( 'NONE', *, *, #8941, .F. ) ;
#8330 = CARTESIAN_POINT ( 'NONE',  ( 131.9330360192018077, -3695.324988468914853, 2260.231623935620519 ) ) ;
#8329 = AXIS2_PLACEMENT_3D ( 'NONE', #20182, #606, #5141 ) ;
#8331 = CALENDAR_DATE ( 2026, 26, 10 ) ;
#8332 = AXIS2_PLACEMENT_3D ( 'NONE', #20479, #4428, #18374 ) ;
#8333 = CARTESIAN_POINT ( 'NONE',  ( -12.69999999999999929, -3663.272340904999965, 2247.392000000000280 ) ) ;
#8334 = CARTESIAN_POINT ( 'NONE',  ( 14.56265065754690191, -3581.645345613470909, 2247.977218229329537 ) ) ;
#8335 = CARTESIAN_POINT ( 'NONE',  ( 134.2762276231818532, -3657.703887669735650, 2245.922900958339142 ) ) ;
#8336 = VECTOR ( 'NONE', #11538, 1000.000000000000000 ) ;
#8337 = VERTEX_POINT ( 'NONE', #7783 ) ;
#8338 = CIRCLE ( 'NONE', #5730, 5.460999999999938126 ) ;
#8339 = CYLINDRICAL_SURFACE ( 'NONE', #12942, 5.714999999998998881 ) ;
#8340 = CARTESIAN_POINT ( 'NONE',  ( 85.29320000000001301, -3594.099999999999909, 2259.837999999999738 ) ) ;
#8341 = ORIENTED_EDGE ( 'NONE', *, *, #5407, .F. ) ;
#8342 = DIRECTION ( 'NONE',  ( 0.000000000000000000, 0.000000000000000000, -1.000000000000000000 ) ) ;
#8343 = AXIS2_PLACEMENT_3D ( 'NONE', #11895, #6055, #869 ) ;
#8344 = APPLIED_DATE_AND_TIME_ASSIGNMENT ( #9507, #16649, ( #4122 ) ) ;
#8345 = AXIS2_PLACEMENT_3D ( 'NONE', #14444, #484, #25 ) ;
#8346 = FACE_OUTER_BOUND ( 'NONE', #4014, .T. ) ;
#8347 = ORIENTED_EDGE ( 'NONE', *, *, #8226, .T. ) ;
#8348 = ORIENTED_EDGE ( 'NONE', *, *, #10587, .F. ) ;
#8349 = LINE ( 'NONE', #8694, #786 ) ;
#8350 = CARTESIAN_POINT ( 'NONE',  ( 161.1088462396999716, -3543.299999999999727, 2279.827800000000025 ) ) ;
#8351 = ORIENTED_EDGE ( 'NONE', *, *, #1108, .F. ) ;
#8352 = CARTESIAN_POINT ( 'NONE',  ( 15.41268679715999923, -3577.928829547000078, 2239.009999999999764 ) ) ;
#8353 = CARTESIAN_POINT ( 'NONE',  ( -12.31899999999994755, -3657.447599999831709, 2247.391999999993914 ) ) ;
#8354 = EDGE_CURVE ( 'NONE', #4174, #2146, #8236, .T. ) ;
#8355 = FACE_OUTER_BOUND ( 'NONE', #8645, .T. ) ;
#8356 = EDGE_CURVE ( 'NONE', #9308, #22211, #15604, .T. ) ;
#8357 = LINE ( 'NONE', #4827, #14870 ) ;
#8358 = AXIS2_PLACEMENT_3D ( 'NONE', #16175, #3288, #9147 ) ;
#8359 = PERSON_AND_ORGANIZATION ( #5446, #1895 ) ;
#8360 = EDGE_CURVE ( 'NONE', #21395, #11858, #16788, .T. ) ;
#8361 = LINE ( 'NONE', #15499, #21571 ) ;
#8362 = FACE_OUTER_BOUND ( 'NONE', #994, .T. ) ;
#8363 = CARTESIAN_POINT ( 'NONE',  ( 127.0000000000000000, -3619.500000000000000, 2260.600000000000364 ) ) ;
#8364 = AXIS2_PLACEMENT_3D ( 'NONE', #17014, #959, #8010 ) ;
#8365 = CARTESIAN_POINT ( 'NONE',  ( 141.6571813405579405, -3657.440126662888360, 2248.289601892444352 ) ) ;
#8366 = ADVANCED_FACE ( 'NONE', ( #11619 ), #13350, .T. ) ;
#8367 = VERTEX_POINT ( 'NONE', #732 ) ;
#8368 = LINE ( 'NONE', #1085, #11462 ) ;
#8369 = VERTEX_POINT ( 'NONE', #6486 ) ;
#8370 = CARTESIAN_POINT ( 'NONE',  ( 12.69999999999999929, -3579.494999999999891, 2246.630000000000109 ) ) ;
#8371 = FACE_OUTER_BOUND ( 'NONE', #7314, .T. ) ;
#8372 = ORIENTED_EDGE ( 'NONE', *, *, #4278, .T. ) ;
#8373 = ORIENTED_EDGE ( 'NONE', *, *, #22559, .F. ) ;
#8374 = CARTESIAN_POINT ( 'NONE',  ( 142.4431999999993366, -3660.383257047431925, 2255.967040000000907 ) ) ;
#8375 = DIRECTION ( 'NONE',  ( -1.000000000000000000, 0.000000000000000000, 0.000000000000000000 ) ) ;
#8376 = DIRECTION ( 'NONE',  ( 0.000000000000000000, -1.000000000000000000, 0.000000000000000000 ) ) ;
#8377 = EDGE_LOOP ( 'NONE', ( #3723, #12643 ) ) ;
#8378 = LINE ( 'NONE', #4854, #8480 ) ;
#8379 = EDGE_CURVE ( 'NONE', #16552, #2161, #4755, .T. ) ;
#8380 = CARTESIAN_POINT ( 'NONE',  ( 116.8400000000000034, -3694.430000000000291, 2247.392000000000280 ) ) ;
#8381 = DIRECTION ( 'NONE',  ( -1.000000000000000000, 0.000000000000000000, 0.000000000000000000 ) ) ;
#8382 = DIRECTION ( 'NONE',  ( -0.8660254037821217832, 0.5000000000040129011, 1.814359422183044529E-12 ) ) ;
#8383 = DIRECTION ( 'NONE',  ( -0.8660254037817188832, 0.5000000000047110094, 3.181634500920069822E-14 ) ) ;
#8384 = EDGE_CURVE ( 'NONE', #20696, #444, #3249, .T. ) ;
#8385 = ORIENTED_EDGE ( 'NONE', *, *, #11518, .F. ) ;
#8386 = APPROVAL_ROLE ( '' ) ;
#8387 = EDGE_CURVE ( 'NONE', #20995, #18145, #21964, .T. ) ;
#8388 = ORIENTED_EDGE ( 'NONE', *, *, #3771, .T. ) ;
#8389 = CARTESIAN_POINT ( 'NONE',  ( 139.6999999999999886, -3579.494999999999891, 2245.359999999999673 ) ) ;
#8390 = VECTOR ( 'NONE', #1030, 1000.000000000000000 ) ;
#8391 = DIRECTION ( 'NONE',  ( 0.000000000000000000, 0.000000000000000000, 1.000000000000000000 ) ) ;
#8392 = CARTESIAN_POINT ( 'NONE',  ( 15.87499999999605116, -3544.061999999999898, 2281.351799999999912 ) ) ;
#8393 = AXIS2_PLACEMENT_3D ( 'NONE', #23142, #8755, #10504 ) ;
#8394 = ORIENTED_EDGE ( 'NONE', *, *, #8124, .F. ) ;
#8395 = CARTESIAN_POINT ( 'NONE',  ( 25.39999999999999858, -3619.500000000000000, 2261.869999999999891 ) ) ;
#8396 = ADVANCED_FACE ( 'NONE', ( #15382 ), #7374, .T. ) ;
#8397 = DIRECTION ( 'NONE',  ( 0.000000000000000000, -1.000000000000000000, 0.000000000000000000 ) ) ;
#8398 = CARTESIAN_POINT ( 'NONE',  ( 144.7204148360012255, -3662.235733769309263, 2245.468189506944327 ) ) ;
#8399 = DIRECTION ( 'NONE',  ( 0.000000000000000000, 0.000000000000000000, -1.000000000000000000 ) ) ;
#8400 = CARTESIAN_POINT ( 'NONE',  ( 12.69999999999999929, -3590.289999999999964, 2268.705139999999574 ) ) ;
#8401 = CARTESIAN_POINT ( 'NONE',  ( 3.175000000003000089, -3544.061999999999898, 2275.001800000000003 ) ) ;
#8402 = VERTEX_POINT ( 'NONE', #14930 ) ;
#8403 = DIRECTION ( 'NONE',  ( 0.000000000000000000, 0.000000000000000000, -1.000000000000000000 ) ) ;
#8404 = AXIS2_PLACEMENT_3D ( 'NONE', #22680, #2062, #16352 ) ;
#8405 = CARTESIAN_POINT ( 'NONE',  ( 34.49320000000000164, -3594.099999999999909, 2239.009999999999764 ) ) ;
#8406 = CIRCLE ( 'NONE', #3160, 0.7619999999999987894 ) ;
#8407 = FACE_OUTER_BOUND ( 'NONE', #18391, .T. ) ;
#8408 = AXIS2_PLACEMENT_3D ( 'NONE', #16918, #654, #2526 ) ;
#8409 = CARTESIAN_POINT ( 'NONE',  ( 10.00572897464999933, -3598.566071899000235, 2279.486249620000308 ) ) ;
#8410 = CARTESIAN_POINT ( 'NONE',  ( 15.54479999999999862, -3639.502500000000055, 2263.571799999999712 ) ) ;
#8411 = ORIENTED_EDGE ( 'NONE', *, *, #2100, .F. ) ;
#8412 = DIRECTION ( 'NONE',  ( 1.000000000000000000, 0.000000000000000000, 0.000000000000000000 ) ) ;
#8413 = VERTEX_POINT ( 'NONE', #13272 ) ;
#8414 = CARTESIAN_POINT ( 'NONE',  ( 9.971028676360534249, -3543.580319128281644, 2255.300887233377580 ) ) ;
#8415 = DATE_AND_TIME ( #7955, #1501 ) ;
#8416 = ADVANCED_FACE ( 'NONE', ( #22061 ), #6030, .T. ) ;
#8417 = FACE_OUTER_BOUND ( 'NONE', #22704, .T. ) ;
#8418 = ADVANCED_FACE ( 'NONE', ( #13396 ), #18551, .T. ) ;
#8419 = CARTESIAN_POINT ( 'NONE',  ( 60.65520000000000067, -3644.899999999999636, 2239.771999999999935 ) ) ;
#8420 = CARTESIAN_POINT ( 'NONE',  ( 9.855199999999999960, -3659.504999999999654, 2272.030000000000200 ) ) ;
#8421 = CIRCLE ( 'NONE', #3170, 11.11250000000000071 ) ;
#8422 = B_SPLINE_CURVE_WITH_KNOTS ( 'NONE', 3,
 ( #9376, #466, #11242, #16748 ),
 .UNSPECIFIED., .F., .F.,
 ( 4, 4 ),
 ( 0.000000000000000000, 1.000000000000000000 ),
 .UNSPECIFIED. ) ;
#8423 = AXIS2_PLACEMENT_3D ( 'NONE', #10789, #8686, #5054 ) ;
#8424 = DIRECTION ( 'NONE',  ( 0.000000000000000000, -1.000000000000000000, 0.000000000000000000 ) ) ;
#8425 = AXIS2_PLACEMENT_3D ( 'NONE', #21436, #12298, #15582 ) ;
#8426 = DIRECTION ( 'NONE',  ( -1.000000000000000000, 0.000000000000000000, 0.000000000000000000 ) ) ;
#8427 = AXIS2_PLACEMENT_3D ( 'NONE', #19619, #21379, #9073 ) ;
#8428 = DIRECTION ( 'NONE',  ( -0.000000000000000000, -1.000000000000000000, -0.000000000000000000 ) ) ;
#8429 = EDGE_CURVE ( 'NONE', #2255, #8201, #272, .T. ) ;
#8430 = ORIENTED_EDGE ( 'NONE', *, *, #22743, .F. ) ;
#8431 = FACE_OUTER_BOUND ( 'NONE', #6347, .T. ) ;
#8432 = CARTESIAN_POINT ( 'NONE',  ( 127.0000000000000000, -3660.140000000000327, 2250.236800000000130 ) ) ;
#8433 = ORIENTED_EDGE ( 'NONE', *, *, #21289, .F. ) ;
#8434 = CARTESIAN_POINT ( 'NONE',  ( 25.39999999999999858, -3670.300000000000182, 2261.869999999999891 ) ) ;
#8435 = DIRECTION ( 'NONE',  ( 1.000000000000000000, 0.000000000000000000, 0.000000000000000000 ) ) ;
#8436 = B_SPLINE_CURVE_WITH_KNOTS ( 'NONE', 3,
 ( #8787, #10424, #5273, #19223 ),
 .UNSPECIFIED., .F., .F.,
 ( 4, 4 ),
 ( 0.000000000000000000, 1.000000000000000000 ),
 .UNSPECIFIED. ) ;
#8437 = EDGE_CURVE ( 'NONE', #19095, #13134, #2610, .T. ) ;
#8438 = VERTEX_POINT ( 'NONE', #8011 ) ;
#8439 = EDGE_CURVE ( 'NONE', #17151, #10571, #999, .T. ) ;
#8440 = ORIENTED_EDGE ( 'NONE', *, *, #4484, .T. ) ;
#8441 = CARTESIAN_POINT ( 'NONE',  ( 139.7000000000063835, -3656.812599999938357, 2239.391000000000076 ) ) ;
#8442 = VECTOR ( 'NONE', #9521, 1000.000000000000000 ) ;
#8443 = AXIS2_PLACEMENT_3D ( 'NONE', #3146, #8552, #15694 ) ;
#8444 = ORIENTED_EDGE ( 'NONE', *, *, #691, .F. ) ;
#8445 = PRODUCT_DEFINITION_SHAPE ( 'NONE', 'NONE',  #1759 ) ;
#8446 = AXIS2_PLACEMENT_3D ( 'NONE', #7480, #229, #19794 ) ;
#8447 = DIRECTION ( 'NONE',  ( 0.000000000000000000, 0.000000000000000000, -1.000000000000000000 ) ) ;
#8448 = DIRECTION ( 'NONE',  ( 0.000000000000000000, 0.000000000000000000, 1.000000000000000000 ) ) ;
#8449 = CIRCLE ( 'NONE', #21547, 6.349999999999855760 ) ;
#8450 = CARTESIAN_POINT ( 'NONE',  ( -0.7620000000000000107, -3694.938000000000102, 2254.250000000000000 ) ) ;
#8451 = ORIENTED_EDGE ( 'NONE', *, *, #18440, .F. ) ;
#8452 = CARTESIAN_POINT ( 'NONE',  ( 131.7911717319573484, -3695.576947737646606, 2259.876481750800394 ) ) ;
#8453 = APPROVAL_STATUS ( 'not_yet_approved' ) ;
#8454 = EDGE_CURVE ( 'NONE', #14892, #3037, #13977, .T. ) ;
#8455 = CARTESIAN_POINT ( 'NONE',  ( 12.70000000005999929, -3576.802599999999984, 2242.820000000000164 ) ) ;
#8456 = CARTESIAN_POINT ( 'NONE',  ( 114.2999999999999972, -3644.899999999999636, 2259.837999999999738 ) ) ;
#8457 = CARTESIAN_POINT ( 'NONE',  ( 134.0212837167035502, -3658.862064473952614, 2244.850302162179105 ) ) ;
#8458 = AXIS2_PLACEMENT_3D ( 'NONE', #2655, #1245, #13207 ) ;
#8459 = EDGE_LOOP ( 'NONE', ( #21239, #1133, #3466, #23089 ) ) ;
#8460 = AXIS2_PLACEMENT_3D ( 'NONE', #8053, #17177, #15317 ) ;
#8461 = DIRECTION ( 'NONE',  ( -2.336881798971000105E-14, 0.000000000000000000, -1.000000000000000000 ) ) ;
#8462 = CIRCLE ( 'NONE', #13691, 2.844799999999999773 ) ;
#8463 = DIRECTION ( 'NONE',  ( 0.000000000000000000, 0.000000000000000000, -1.000000000000000000 ) ) ;
#8464 = ORIENTED_EDGE ( 'NONE', *, *, #6716, .F. ) ;
#8465 = CYLINDRICAL_SURFACE ( 'NONE', #7250, 2.844800000000001550 ) ;
#8466 = CIRCLE ( 'NONE', #8851, 0.7619999999999987894 ) ;
#8467 = ORIENTED_EDGE ( 'NONE', *, *, #20404, .T. ) ;
#8468 = AXIS2_PLACEMENT_3D ( 'NONE', #1192, #13506, #4600 ) ;
#8469 = CARTESIAN_POINT ( 'NONE',  ( 151.4000000000000057, -3543.299999999999727, 2295.829799999999977 ) ) ;
#8470 = FACE_OUTER_BOUND ( 'NONE', #12777, .T. ) ;
#8471 = ORIENTED_EDGE ( 'NONE', *, *, #14607, .F. ) ;
#8472 = CARTESIAN_POINT ( 'NONE',  ( 0.7620000000000000107, -3694.938000000000102, 2295.829799999999977 ) ) ;
#8473 = FACE_OUTER_BOUND ( 'NONE', #153, .T. ) ;
#8474 = DIRECTION ( 'NONE',  ( 0.000000000000000000, 0.000000000000000000, -1.000000000000000000 ) ) ;
#8475 = AXIS2_PLACEMENT_3D ( 'NONE', #17036, #6283, #15065 ) ;
#8476 = CIRCLE ( 'NONE', #4300, 0.7619999999999294005 ) ;
#8477 = DIRECTION ( 'NONE',  ( -0.7071067811865969777, 0.000000000000000000, -0.7071067811864980568 ) ) ;
#8478 = PERSON_AND_ORGANIZATION ( #5446, #1895 ) ;
#8479 = EDGE_LOOP ( 'NONE', ( #19302, #9203 ) ) ;
#8480 = VECTOR ( 'NONE', #22659, 1000.000000000000000 ) ;
#8481 = CARTESIAN_POINT ( 'NONE',  ( 88.90000000000000568, -3644.899999999999636, 2259.837999999999738 ) ) ;
#8482 = DIRECTION ( 'NONE',  ( 2.324635735433000053E-14, 0.000000000000000000, 1.000000000000000000 ) ) ;
#8483 = CARTESIAN_POINT ( 'NONE',  ( 18.41499991942999159, -3579.609095813635122, 2244.645121672054302 ) ) ;
#8484 =( BOUNDED_CURVE ( )  B_SPLINE_CURVE ( 3, ( #18645, #13375, #16657, #20516 ),
 .UNSPECIFIED., .F., .F. ) 
 B_SPLINE_CURVE_WITH_KNOTS ( ( 4, 4 ),
 ( 4.620504083482610562E-16, 1.570796326138795385 ),
 .UNSPECIFIED. ) 
 CURVE ( )  GEOMETRIC_REPRESENTATION_ITEM ( )  RATIONAL_B_SPLINE_CURVE ( ( 1.000000000000000000, 0.8047378542790095679, 0.8047378542790095679, 1.000000000000000000 ) ) 
 REPRESENTATION_ITEM ( '' )  );
#8485 = CIRCLE ( 'NONE', #3236, 0.7619999999999987894 ) ;
#8486 = CARTESIAN_POINT ( 'NONE',  ( 142.0943346817877284, -3657.968795034299546, 2249.230143411615245 ) ) ;
#8487 = ORIENTED_EDGE ( 'NONE', *, *, #3853, .T. ) ;
#8488 = FACE_OUTER_BOUND ( 'NONE', #1886, .T. ) ;
#8489 = ADVANCED_FACE ( 'NONE', ( #19134 ), #19366, .F. ) ;
#8490 = ORIENTED_EDGE ( 'NONE', *, *, #15719, .T. ) ;
#8491 = CIRCLE ( 'NONE', #9249, 0.7619999999999294005 ) ;
#8492 = DIRECTION ( 'NONE',  ( 1.000000000000000000, 0.000000000000000000, 0.000000000000000000 ) ) ;
#8493 = EDGE_LOOP ( 'NONE', ( #17581, #18803, #5695, #20834 ) ) ;
#8494 = ORIENTED_EDGE ( 'NONE', *, *, #14031, .F. ) ;
#8495 = CARTESIAN_POINT ( 'NONE',  ( 4.806249414519654373, -3543.438632180929289, 2259.914298575651628 ) ) ;
#8496 = CARTESIAN_POINT ( 'NONE',  ( 151.4000000000000057, -3695.670967364599164, 2240.279999999999745 ) ) ;
#8497 = CIRCLE ( 'NONE', #21602, 2.844799999999994444 ) ;
#8498 = CARTESIAN_POINT ( 'NONE',  ( 137.1599999999999966, -3660.786127253999894, 2255.774000000000342 ) ) ;
#8499 = VERTEX_POINT ( 'NONE', #14096 ) ;
#8500 = TOROIDAL_SURFACE ( 'NONE', #16720, 1.905000000000000027, 1.270000000000000018 ) ;
#8501 = DIRECTION ( 'NONE',  ( 0.000000000000000000, 0.000000000000000000, -1.000000000000000000 ) ) ;
#8502 = CARTESIAN_POINT ( 'NONE',  ( 139.6999999999999886, -3657.599999999999909, 2270.760000000000218 ) ) ;
#8503 = CIRCLE ( 'NONE', #1383, 5.079999999999973426 ) ;
#8504 = CYLINDRICAL_SURFACE ( 'NONE', #11721, 0.3809999999999154618 ) ;
#8505 = FACE_OUTER_BOUND ( 'NONE', #5759, .T. ) ;
#8506 = ORIENTED_EDGE ( 'NONE', *, *, #17722, .F. ) ;
#8507 = DATE_TIME_ROLE ( 'classification_date' ) ;
#8508 = CARTESIAN_POINT ( 'NONE',  ( 12.70000000005999929, -3576.362659094999799, 2239.009999999999764 ) ) ;
#8509 = APPLIED_PERSON_AND_ORGANIZATION_ASSIGNMENT ( #12736, #10308, ( #7499 ) ) ;
#8510 = DIRECTION ( 'NONE',  ( -1.000000000000000000, 0.000000000000000000, 0.000000000000000000 ) ) ;
#8511 = AXIS2_PLACEMENT_3D ( 'NONE', #3280, #1163, #3157 ) ;
#8512 = DIRECTION ( 'NONE',  ( 0.000000000000000000, 1.000000000000000000, 0.000000000000000000 ) ) ;
#8513 = ADVANCED_BREP_SHAPE_REPRESENTATION ( '', ( #13479, #5611 ), #12354 ) ;
#8514 = EDGE_LOOP ( 'NONE', ( #8007, #18376, #21619, #16421 ) ) ;
#8515 = FACE_BOUND ( 'NONE', #11247, .T. ) ;
#8516 = EDGE_CURVE ( 'NONE', #3779, #6730, #8491, .T. ) ;
#8517 = TOROIDAL_SURFACE ( 'NONE', #17115, 5.080000000000000071, 0.3810000000000000053 ) ;
#8518 = ADVANCED_FACE ( 'NONE', ( #21129 ), #14113, .T. ) ;
#8519 = VECTOR ( 'NONE', #5039, 1000.000000000000000 ) ;
#8520 = DIRECTION ( 'NONE',  ( 0.000000000000000000, 0.000000000000000000, 1.000000000000000000 ) ) ;
#8521 = CARTESIAN_POINT ( 'NONE',  ( 144.6523069729103099, -3662.357674682753895, 2245.609748382597900 ) ) ;
#8522 = DIRECTION ( 'NONE',  ( -0.5000000000007065459, 0.8660254037840305896, 0.000000000000000000 ) ) ;
#8523 = CARTESIAN_POINT ( 'NONE',  ( 11.52540003424859982, -3662.096080434181204, 2249.457718961763021 ) ) ;
#8524 = EDGE_CURVE ( 'NONE', #9973, #20183, #13729, .T. ) ;
#8525 = CARTESIAN_POINT ( 'NONE',  ( 147.3199999999999932, -3544.570000000000164, 2260.600000000000364 ) ) ;
#8526 = ORIENTED_EDGE ( 'NONE', *, *, #19094, .T. ) ;
#8527 = LINE ( 'NONE', #22688, #6542 ) ;
#8528 = FACE_OUTER_BOUND ( 'NONE', #7775, .T. ) ;
#8529 = AXIS2_PLACEMENT_3D ( 'NONE', #13340, #18494, #6320 ) ;
#8530 = DIRECTION ( 'NONE',  ( 0.000000000000000000, 0.000000000000000000, 1.000000000000000000 ) ) ;
#8531 = CARTESIAN_POINT ( 'NONE',  ( 15.09459832061900464, -3657.969225429738799, 2249.230664226648514 ) ) ;
#8532 = DIRECTION ( 'NONE',  ( 0.000000000000000000, 0.000000000000000000, 1.000000000000000000 ) ) ;
#8533 = VERTEX_POINT ( 'NONE', #10576 ) ;
#8534 = ADVANCED_FACE ( 'NONE', ( #5071 ), #22753, .F. ) ;
#8535 = ORIENTED_EDGE ( 'NONE', *, *, #2128, .F. ) ;
#8536 = VECTOR ( 'NONE', #17141, 1000.000000000000000 ) ;
#8537 = LINE ( 'NONE', #1482, #1972 ) ;
#8538 = EDGE_CURVE ( 'NONE', #17318, #22471, #22399, .T. ) ;
#8539 = VERTEX_POINT ( 'NONE', #5193 ) ;
#8540 = CARTESIAN_POINT ( 'NONE',  ( 12.69999261053000872, -3636.657698770683055, 2279.817639764992691 ) ) ;
#8541 = DATE_AND_TIME ( #15914, #12754 ) ;
#8542 = FACE_OUTER_BOUND ( 'NONE', #19845, .T. ) ;
#8543 = ORIENTED_EDGE ( 'NONE', *, *, #13450, .F. ) ;
#8544 = CARTESIAN_POINT ( 'NONE',  ( 140.0750197493808855, -3576.668786553544578, 2257.597441013394473 ) ) ;
#8545 = CARTESIAN_POINT ( 'NONE',  ( 1.270000000000000018, -3660.140000000000327, 2243.277199999999993 ) ) ;
#8546 = CARTESIAN_POINT ( 'NONE',  ( 12.70000000000000462, -3596.652698770568804, 2279.817639764978139 ) ) ;
#8547 = CARTESIAN_POINT ( 'NONE',  ( 152.4000000000000057, -3694.938000000000102, 2280.589800000000196 ) ) ;
#8548 = DIRECTION ( 'NONE',  ( 0.000000000000000000, 0.000000000000000000, 1.000000000000000000 ) ) ;
#8549 = VERTEX_POINT ( 'NONE', #17247 ) ;
#8550 = CYLINDRICAL_SURFACE ( 'NONE', #20795, 2.844800000000001550 ) ;
#8551 = ADVANCED_FACE ( 'NONE', ( #8587 ), #1309, .F. ) ;
#8552 = DIRECTION ( 'NONE',  ( 3.194481088216070180E-14, 0.5000000000047110094, 0.8660254037817188832 ) ) ;
#8553 = ORIENTED_EDGE ( 'NONE', *, *, #577, .F. ) ;
#8554 = CARTESIAN_POINT ( 'NONE',  ( 136.8551930557000276, -3659.505009668000184, 2250.165028799000083 ) ) ;
#8555 = CARTESIAN_POINT ( 'NONE',  ( 10.68379541473369976, -3657.497568268327541, 2248.446992609373410 ) ) ;
#8556 = EDGE_CURVE ( 'NONE', #16324, #2966, #2882, .T. ) ;
#8557 = EDGE_CURVE ( 'NONE', #9431, #7940, #2956, .T. ) ;
#8558 = EDGE_LOOP ( 'NONE', ( #8598, #8137, #15346, #13736 ) ) ;
#8559 = CARTESIAN_POINT ( 'NONE',  ( 134.3605230499748302, -3581.533682376092202, 2246.411846944817171 ) ) ;
#8560 = VERTEX_POINT ( 'NONE', #6721 ) ;
#8561 = CARTESIAN_POINT ( 'NONE',  ( 15.24000000000000021, -3580.776127254000130, 2255.774000000000342 ) ) ;
#8562 = PERSON_AND_ORGANIZATION_ROLE ( 'creator' ) ;
#8563 = DIRECTION ( 'NONE',  ( -0.7249994335944036639, 0.000000000000000000, -0.6887494619147036534 ) ) ;
#8564 = ORIENTED_EDGE ( 'NONE', *, *, #14591, .T. ) ;
#8565 = AXIS2_PLACEMENT_3D ( 'NONE', #10886, #1751, #8901 ) ;
#8566 = CARTESIAN_POINT ( 'NONE',  ( 136.9464494900593934, -3580.233491490071174, 2257.939127522359740 ) ) ;
#8567 = PERSON_AND_ORGANIZATION ( #5446, #1895 ) ;
#8568 = CARTESIAN_POINT ( 'NONE',  ( 6.222999999999998977, -3659.504999999999654, 2239.771999999999935 ) ) ;
#8569 = CARTESIAN_POINT ( 'NONE',  ( 15.39964945764670645, -3580.393900429462519, 2249.788766634620060 ) ) ;
#8570 = EDGE_CURVE ( 'NONE', #13091, #10412, #4719, .T. ) ;
#8571 = CARTESIAN_POINT ( 'NONE',  ( 133.9850000806000025, -3659.504501929000071, 2244.618659328000376 ) ) ;
#8572 = DIRECTION ( 'NONE',  ( 0.000000000000000000, 1.000000000000000000, 0.000000000000000000 ) ) ;
#8573 = VERTEX_POINT ( 'NONE', #7070 ) ;
#8574 = CARTESIAN_POINT ( 'NONE',  ( 12.69999999999999929, -3576.650200000000041, 2257.592639999999847 ) ) ;
#8575 = ORIENTED_EDGE ( 'NONE', *, *, #9547, .F. ) ;
#8576 = AXIS2_PLACEMENT_3D ( 'NONE', #20225, #3939, #11094 ) ;
#8577 = DIRECTION ( 'NONE',  ( 0.000000000000000000, 1.000000000000000000, 0.000000000000000000 ) ) ;
#8578 = EDGE_CURVE ( 'NONE', #20939, #17497, #8357, .T. ) ;
#8579 = CARTESIAN_POINT ( 'NONE',  ( 15.03168679714000078, -3598.151299999999992, 2292.781800000000203 ) ) ;
#8580 = ORIENTED_EDGE ( 'NONE', *, *, #22888, .F. ) ;
#8581 = CARTESIAN_POINT ( 'NONE',  ( 12.69999999999999929, -3648.710000000000036, 2268.705139999999574 ) ) ;
#8582 = CARTESIAN_POINT ( 'NONE',  ( 57.14999999999999858, -3670.300000000000182, 2247.392000000000280 ) ) ;
#8583 = VERTEX_POINT ( 'NONE', #17356 ) ;
#8584 = DIRECTION ( 'NONE',  ( 0.000000000000000000, 0.000000000000000000, 1.000000000000000000 ) ) ;
#8585 = DIRECTION ( 'NONE',  ( -1.000000000000000000, 0.000000000000000000, 0.000000000000000000 ) ) ;
#8586 = CARTESIAN_POINT ( 'NONE',  ( 127.0000000000000000, -3660.140000000000327, 2247.392000000000280 ) ) ;
#8587 = FACE_OUTER_BOUND ( 'NONE', #56, .T. ) ;
#8588 = APPROVAL_STATUS ( 'not_yet_approved' ) ;
#8589 = CARTESIAN_POINT ( 'NONE',  ( 15.87499999999605116, -3544.061999999999898, 2281.351799999999912 ) ) ;
#8590 = CARTESIAN_POINT ( 'NONE',  ( 1.270000000000000018, -3660.140000000000327, 2251.506800000000112 ) ) ;
#8591 = CARTESIAN_POINT ( 'NONE',  ( 18.38859181429490519, -3580.043763408477844, 2244.804994013233681 ) ) ;
#8592 = AXIS2_PLACEMENT_3D ( 'NONE', #15876, #5219, #10944 ) ;
#8593 = EDGE_CURVE ( 'NONE', #10141, #22306, #11981, .T. ) ;
#8594 = EDGE_CURVE ( 'NONE', #15748, #13823, #17840, .T. ) ;
#8595 = CARTESIAN_POINT ( 'NONE',  ( 141.5264891900619659, -3657.323731859511554, 2246.960912804729105 ) ) ;
#8596 = ORIENTED_EDGE ( 'NONE', *, *, #17718, .T. ) ;
#8597 = DIRECTION ( 'NONE',  ( 0.000000000000000000, 0.000000000000000000, -1.000000000000000000 ) ) ;
#8598 = ORIENTED_EDGE ( 'NONE', *, *, #16012, .F. ) ;
#8599 = VERTEX_POINT ( 'NONE', #1432 ) ;
#8600 = ORIENTED_EDGE ( 'NONE', *, *, #12089, .T. ) ;
#8601 = LINE ( 'NONE', #22649, #2431 ) ;
#8602 = ORIENTED_EDGE ( 'NONE', *, *, #16811, .F. ) ;
#8603 = ORIENTED_EDGE ( 'NONE', *, *, #17722, .T. ) ;
#8604 = B_SPLINE_CURVE_WITH_KNOTS ( 'NONE', 3,
 ( #18797, #16920, #2527, #22537, #20449, #6162, #986, #6052, #4620, #1096, #8030, #15292, #13416, #865, #11759, #18682, #2868 ),
 .UNSPECIFIED., .F., .F.,
 ( 4, 1, 1, 1, 1, 1, 1, 1, 1, 1, 1, 1, 1, 1, 4 ),
 ( 0.000000000000000000, 0.07142857142856999519, 0.1428571428570999946, 0.2142857142857000075, 0.2857142857143000203, 0.3571428571429000054, 0.4285714285713999594, 0.5000000000000000000, 0.5714285714286000406, 0.6428571428570999391, 0.7142857142856999797, 0.7857142857142999093, 0.8571428571429000609, 0.9285714285714000704, 1.000000000000000000 ),
 .UNSPECIFIED. ) ;
#8605 = LOCAL_TIME ( 17, 37, 43.00000000000000000, #10221 ) ;
#8606 = DIRECTION ( 'NONE',  ( -0.7071067811865691111, 0.000000000000000000, 0.7071067811865258124 ) ) ;
#8607 = CONTEXT_DEPENDENT_SHAPE_REPRESENTATION ( #18475, #21746 ) ;
#8608 = CARTESIAN_POINT ( 'NONE',  ( 127.0000000000000000, -3660.140000000000327, 2250.236800000000130 ) ) ;
#8609 = AXIS2_PLACEMENT_3D ( 'NONE', #9397, #16531, #486 ) ;
#8610 = CARTESIAN_POINT ( 'NONE',  ( 18.37960467573999779, -3578.859731361000286, 2244.547525601999951 ) ) ;
#8611 = ORIENTED_EDGE ( 'NONE', *, *, #4965, .F. ) ;
#8612 = CARTESIAN_POINT ( 'NONE',  ( 137.1599999999999966, -3578.213872745999652, 2255.774000000000342 ) ) ;
#8613 = CARTESIAN_POINT ( 'NONE',  ( 59.89320000000000022, -3644.899999999999636, 2260.600000000000364 ) ) ;
#8614 = DIRECTION ( 'NONE',  ( 0.000000000000000000, 0.000000000000000000, -1.000000000000000000 ) ) ;
#8615 = SHAPE_REPRESENTATION ( 'Screw 1', ( #5611 ), #12354 ) ;
#8616 = DIRECTION ( 'NONE',  ( 1.000000000000000000, 0.000000000000000000, 0.000000000000000000 ) ) ;
#8617 = ORIENTED_EDGE ( 'NONE', *, *, #22408, .T. ) ;
#8618 = PERSON_AND_ORGANIZATION ( #5446, #1895 ) ;
#8619 = CARTESIAN_POINT ( 'NONE',  ( -5.588000000000000078, -3694.938000000000102, 2254.250000000000000 ) ) ;
#8620 = AXIS2_PLACEMENT_3D ( 'NONE', #11321, #7581, #11107 ) ;
#8621 = CARTESIAN_POINT ( 'NONE',  ( 10.06389858027753448, -3580.564515547758219, 2249.669647745964994 ) ) ;
#8622 = DIRECTION ( 'NONE',  ( 1.000000000000000000, 0.000000000000000000, 0.000000000000000000 ) ) ;
#8623 = LOCAL_TIME ( 17, 37, 43.00000000000000000, #2225 ) ;
#8624 = AXIS2_PLACEMENT_3D ( 'NONE', #6458, #19101, #8325 ) ;
#8625 = ORIENTED_EDGE ( 'NONE', *, *, #7556, .T. ) ;
#8626 = AXIS2_PLACEMENT_3D ( 'NONE', #22859, #22978, #6835 ) ;
#8627 = DIRECTION ( 'NONE',  ( 0.000000000000000000, 0.000000000000000000, 1.000000000000000000 ) ) ;
#8628 = DIRECTION ( 'NONE',  ( 1.000000000000000000, 0.000000000000000000, 0.000000000000000000 ) ) ;
#8629 = CARTESIAN_POINT ( 'NONE',  ( 131.9679793872000175, -3694.678775005999796, 2260.577432963000319 ) ) ;
#8630 = CARTESIAN_POINT ( 'NONE',  ( 9.990450446634426385, -3660.417187683251086, 2250.236801297000056 ) ) ;
#8631 = DIRECTION ( 'NONE',  ( 0.000000000000000000, 1.000000000000000000, 0.000000000000000000 ) ) ;
#8632 = ORIENTED_EDGE ( 'NONE', *, *, #4435, .T. ) ;
#8633 = DIRECTION ( 'NONE',  ( 0.000000000000000000, 0.000000000000000000, -1.000000000000000000 ) ) ;
#8634 = LINE ( 'NONE', #6771, #13686 ) ;
#8635 = APPLIED_DATE_AND_TIME_ASSIGNMENT ( #17017, #22862, ( #17188 ) ) ;
#8636 = CARTESIAN_POINT ( 'NONE',  ( 116.8400000000000034, -3694.430000000000291, 2247.392000000000280 ) ) ;
#8637 = DIRECTION ( 'NONE',  ( 0.000000000000000000, 0.000000000000000000, -1.000000000000000000 ) ) ;
#8638 = DIRECTION ( 'NONE',  ( -1.729311324296000017E-12, 1.000000000000000000, -3.793660610079000032E-12 ) ) ;
#8639 = APPROVAL_PERSON_ORGANIZATION ( #22810, #16776, #5251 ) ;
#8640 = APPROVAL_PERSON_ORGANIZATION ( #4173, #2619, #14959 ) ;
#8641 = ORIENTED_EDGE ( 'NONE', *, *, #4360, .T. ) ;
#8642 = EDGE_CURVE ( 'NONE', #15975, #7394, #6625, .T. ) ;
#8643 = CARTESIAN_POINT ( 'NONE',  ( 20.32000000000000028, -3543.299999999999727, 2292.819899999999961 ) ) ;
#8644 = EDGE_CURVE ( 'NONE', #16167, #7890, #12564, .T. ) ;
#8645 = EDGE_LOOP ( 'NONE', ( #13357, #20838, #4383, #10589 ) ) ;
#8646 = CARTESIAN_POINT ( 'NONE',  ( 13.78126912685999983, -3582.131243251999877, 2257.644351290000031 ) ) ;
#8647 = PERSON_AND_ORGANIZATION ( #15771, #13132 ) ;
#8648 = EDGE_CURVE ( 'NONE', #2498, #3774, #7033, .T. ) ;
#8649 = AXIS2_PLACEMENT_3D ( 'NONE', #9070, #3783, #9309 ) ;
#8650 = DIRECTION ( 'NONE',  ( 1.000000000000000000, 0.000000000000000000, 0.000000000000000000 ) ) ;
#8651 = FACE_OUTER_BOUND ( 'NONE', #13615, .T. ) ;
#8652 = DIRECTION ( 'NONE',  ( -0.5000000000043351989, -0.8660254037819355988, 0.000000000000000000 ) ) ;
#8653 = DIRECTION ( 'NONE',  ( 0.000000000000000000, 0.000000000000000000, -1.000000000000000000 ) ) ;
#8654 = CARTESIAN_POINT ( 'NONE',  ( 17.33724445481948706, -3576.154475310671842, 2246.502948247453787 ) ) ;
#8655 = ADVANCED_FACE ( 'NONE', ( #12449 ), #19597, .T. ) ;
#8656 = LOCAL_TIME ( 17, 37, 43.00000000000000000, #3674 ) ;
#8657 = CARTESIAN_POINT ( 'NONE',  ( 0.7620000000000000107, -3544.061999999999898, 2275.001800000000003 ) ) ;
#8658 = ORIENTED_EDGE ( 'NONE', *, *, #3381, .F. ) ;
#8659 = DIRECTION ( 'NONE',  ( 0.000000000000000000, 0.000000000000000000, 1.000000000000000000 ) ) ;
#8660 = DIRECTION ( 'NONE',  ( 0.000000000000000000, 0.000000000000000000, -1.000000000000000000 ) ) ;
#8661 = ORIENTED_EDGE ( 'NONE', *, *, #6105, .T. ) ;
#8662 = EDGE_CURVE ( 'NONE', #16167, #7575, #10000, .T. ) ;
#8663 = LINE ( 'NONE', #5157, #3174 ) ;
#8664 = DIRECTION ( 'NONE',  ( -0.8928571428563309986, 0.4503400076058416968, 0.000000000000000000 ) ) ;
#8665 = VECTOR ( 'NONE', #2989, 1000.000000000000000 ) ;
#8666 = ORIENTED_EDGE ( 'NONE', *, *, #6930, .F. ) ;
#8667 = DIRECTION ( 'NONE',  ( 1.000000000000000000, 0.000000000000000000, 0.000000000000000000 ) ) ;
#8668 = ORIENTED_EDGE ( 'NONE', *, *, #9941, .F. ) ;
#8669 = ORIENTED_EDGE ( 'NONE', *, *, #13042, .F. ) ;
#8670 = DIRECTION ( 'NONE',  ( -1.000000000000000000, 0.000000000000000000, 0.000000000000000000 ) ) ;
#8671 = PERSON_AND_ORGANIZATION ( #5446, #1895 ) ;
#8672 = FACE_OUTER_BOUND ( 'NONE', #4751, .T. ) ;
#8673 = EDGE_CURVE ( 'NONE', #9684, #12626, #15251, .T. ) ;
#8674 = ORIENTED_EDGE ( 'NONE', *, *, #14428, .T. ) ;
#8675 = CARTESIAN_POINT ( 'NONE',  ( 106.0884186392999879, -3694.938000000000102, 2323.750833010999941 ) ) ;
#8676 = ADVANCED_FACE ( 'NONE', ( #12910 ), #643, .T. ) ;
#8677 = PERSON_AND_ORGANIZATION_ROLE ( 'creator' ) ;
#8678 = EDGE_CURVE ( 'NONE', #6472, #19890, #1012, .T. ) ;
#8679 = CARTESIAN_POINT ( 'NONE',  ( 15.37455142657321083, -3580.464775575591375, 2249.741195994737609 ) ) ;
#8680 = VECTOR ( 'NONE', #636, 1000.000000000000000 ) ;
#8681 = FACE_OUTER_BOUND ( 'NONE', #12388, .T. ) ;
#8682 = FACE_OUTER_BOUND ( 'NONE', #17763, .T. ) ;
#8683 = DIRECTION ( 'NONE',  ( 0.000000000000000000, 0.000000000000000000, -1.000000000000000000 ) ) ;
#8684 = ORIENTED_EDGE ( 'NONE', *, *, #20102, .F. ) ;
#8685 = CARTESIAN_POINT ( 'NONE',  ( 15.39361733587799819, -3695.340677397469335, 2255.389245125670186 ) ) ;
#8686 = DIRECTION ( 'NONE',  ( 0.000000000000000000, 0.000000000000000000, 1.000000000000000000 ) ) ;
#8687 = ORIENTED_EDGE ( 'NONE', *, *, #7280, .T. ) ;
#8688 = EDGE_CURVE ( 'NONE', #1252, #14593, #7295, .T. ) ;
#8689 = CARTESIAN_POINT ( 'NONE',  ( 101.5999999999999943, -3568.700000000000273, 2260.600000000000364 ) ) ;
#8690 = AXIS2_PLACEMENT_3D ( 'NONE', #11213, #18243, #5609 ) ;
#8691 = DIRECTION ( 'NONE',  ( 0.000000000000000000, 1.000000000000000000, 0.000000000000000000 ) ) ;
#8692 = ORIENTED_EDGE ( 'NONE', *, *, #21603, .F. ) ;
#8693 = ORIENTED_EDGE ( 'NONE', *, *, #21895, .F. ) ;
#8694 = CARTESIAN_POINT ( 'NONE',  ( 98.75520000000000209, -3670.300000000000182, 2261.869999999999891 ) ) ;
#8695 = VECTOR ( 'NONE', #5549, 1000.000000000000114 ) ;
#8696 = FACE_BOUND ( 'NONE', #20678, .T. ) ;
#8697 = AXIS2_PLACEMENT_3D ( 'NONE', #2783, #16426, #9928 ) ;
#8698 = ORIENTED_EDGE ( 'NONE', *, *, #10304, .T. ) ;
#8699 = AXIS2_PLACEMENT_3D ( 'NONE', #20702, #8532, #1015 ) ;
#8700 = DIRECTION ( 'NONE',  ( 0.000000000000000000, 0.000000000000000000, 1.000000000000000000 ) ) ;
#8701 = DIRECTION ( 'NONE',  ( 0.000000000000000000, 0.000000000000000000, 1.000000000000000000 ) ) ;
#8702 = CARTESIAN_POINT ( 'NONE',  ( 15.54479999999999862, -3599.602668064999762, 2279.447335734999797 ) ) ;
#8703 = DIRECTION ( 'NONE',  ( 1.000000000000000000, 0.000000000000000000, 0.000000000000000000 ) ) ;
#8704 = APPROVAL_DATE_TIME ( #5194, #18651 ) ;
#8705 = LINE ( 'NONE', #12684, #5917 ) ;
#8706 = CARTESIAN_POINT ( 'NONE',  ( 9.886249413367808714, -3695.561367819954285, 2255.088298574058626 ) ) ;
#8707 = CARTESIAN_POINT ( 'NONE',  ( 18.31792581816387155, -3580.544012085188569, 2245.098288300677268 ) ) ;
#8708 = CIRCLE ( 'NONE', #3833, 1.240967364599221412 ) ;
#8709 = ADVANCED_FACE ( 'NONE', ( #10803 ), #17944, .F. ) ;
#8710 = CARTESIAN_POINT ( 'NONE',  ( 142.1023807964371883, -3657.981398713484396, 2249.244952485364138 ) ) ;
#8711 = ADVANCED_FACE ( 'NONE', ( #14333, #3762 ), #1896, .T. ) ;
#8712 = EDGE_CURVE ( 'NONE', #19931, #3802, #3334, .T. ) ;
#8713 = VERTEX_POINT ( 'NONE', #16422 ) ;
#8714 = VECTOR ( 'NONE', #9777, 1000.000000000000000 ) ;
#8715 = DIRECTION ( 'NONE',  ( 0.000000000000000000, 0.000000000000000000, -1.000000000000000000 ) ) ;
#8716 = AXIS2_PLACEMENT_3D ( 'NONE', #3942, #11864, #12849 ) ;
#8717 = ORIENTED_EDGE ( 'NONE', *, *, #20734, .T. ) ;
#8718 = ORIENTED_EDGE ( 'NONE', *, *, #21851, .F. ) ;
#8719 = ADVANCED_FACE ( 'NONE', ( #18068 ), #16078, .T. ) ;
#8720 = ORIENTED_EDGE ( 'NONE', *, *, #3938, .F. ) ;
#8721 = CIRCLE ( 'NONE', #21819, 0.3809999999999647002 ) ;
#8722 = DIRECTION ( 'NONE',  ( -2.324635735433000053E-14, 0.000000000000000000, -1.000000000000000000 ) ) ;
#8723 = ORIENTED_EDGE ( 'NONE', *, *, #6930, .T. ) ;
#8724 = EDGE_LOOP ( 'NONE', ( #19033, #8291, #16208, #21003 ) ) ;
#8725 = CARTESIAN_POINT ( 'NONE',  ( 4.931826670915151034, -3543.672816123386383, 2260.228926848877109 ) ) ;
#8726 = DATE_AND_TIME ( #19499, #11611 ) ;
#8727 = CARTESIAN_POINT ( 'NONE',  ( 139.7000000000001876, -3582.670000000000073, 2245.359999999999673 ) ) ;
#8728 = CIRCLE ( 'NONE', #17696, 2.844799999998995244 ) ;
#8729 = DIRECTION ( 'NONE',  ( -1.000000000000000000, 0.000000000000000000, 0.000000000000000000 ) ) ;
#8730 = EDGE_CURVE ( 'NONE', #2777, #19095, #8138, .T. ) ;
#8731 = VERTEX_POINT ( 'NONE', #20070 ) ;
#8732 = DIRECTION ( 'NONE',  ( -0.5000000000043488546, -0.8660254037819278272, 0.000000000000000000 ) ) ;
#8733 = EDGE_CURVE ( 'NONE', #4102, #3518, #20850, .T. ) ;
#8734 = DIRECTION ( 'NONE',  ( 0.7071067811865691111, 0.000000000000000000, 0.7071067811865258124 ) ) ;
#8735 = AXIS2_PLACEMENT_3D ( 'NONE', #6260, #4595, #9867 ) ;
#8736 = DIRECTION ( 'NONE',  ( -1.000000000000000000, 0.000000000000000000, 0.000000000000000000 ) ) ;
#8737 = ORIENTED_EDGE ( 'NONE', *, *, #2841, .F. ) ;
#8738 = PERSON_AND_ORGANIZATION ( #5446, #1895 ) ;
#8739 = VECTOR ( 'NONE', #9157, 999.9999999999998863 ) ;
#8740 = CARTESIAN_POINT ( 'NONE',  ( 131.8995956651736208, -3543.598402616399198, 2260.148194448883260 ) ) ;
#8741 = CARTESIAN_POINT ( 'NONE',  ( 10.31198979717081343, -3581.040930137735813, 2249.218597259193757 ) ) ;
#8742 = EDGE_CURVE ( 'NONE', #15879, #4712, #22337, .T. ) ;
#8743 = DIRECTION ( 'NONE',  ( 0.000000000000000000, 0.000000000000000000, 1.000000000000000000 ) ) ;
#8744 = EDGE_LOOP ( 'NONE', ( #5066, #12430, #5846, #5742 ) ) ;
#8745 = AXIS2_PLACEMENT_3D ( 'NONE', #4901, #20598, #20491 ) ;
#8746 = FACE_OUTER_BOUND ( 'NONE', #10693, .T. ) ;
#8747 = VECTOR ( 'NONE', #4507, 1000.000000000000000 ) ;
#8748 = CARTESIAN_POINT ( 'NONE',  ( -6.730999999999872863, -3578.860000000000127, 2252.853000000000065 ) ) ;
#8749 = FACE_BOUND ( 'NONE', #14273, .T. ) ;
#8750 = CARTESIAN_POINT ( 'NONE',  ( 1.270000000000000018, -3543.299999999999727, 2240.279999999999745 ) ) ;
#8751 = CARTESIAN_POINT ( 'NONE',  ( 12.06527293566236203, -3662.278322999314241, 2249.268379514652679 ) ) ;
#8752 = VECTOR ( 'NONE', #21347, 1000.000000000000000 ) ;
#8753 = CARTESIAN_POINT ( 'NONE',  ( 10.16000000000000014, -3658.223872745999870, 2255.774000000000342 ) ) ;
#8754 = ORIENTED_EDGE ( 'NONE', *, *, #22802, .F. ) ;
#8755 = DIRECTION ( 'NONE',  ( 0.000000000000000000, 2.336881798971000105E-14, -1.000000000000000000 ) ) ;
#8756 =( BOUNDED_CURVE ( )  B_SPLINE_CURVE ( 3, ( #6604, #22626, #1303, #22747 ),
 .UNSPECIFIED., .F., .F. ) 
 B_SPLINE_CURVE_WITH_KNOTS ( ( 4, 4 ),
 ( 3.673835071120113713E-14, 1.570796327042234264 ),
 .UNSPECIFIED. ) 
 CURVE ( )  GEOMETRIC_REPRESENTATION_ITEM ( )  RATIONAL_B_SPLINE_CURVE ( ( 1.000000000000000000, 0.8047378540660755641, 0.8047378540660755641, 1.000000000000000000 ) ) 
 REPRESENTATION_ITEM ( '' )  );
#8757 = CARTESIAN_POINT ( 'NONE',  ( 12.69999999999999929, -3668.712499999999636, 2268.705139999999574 ) ) ;
#8758 = CARTESIAN_POINT ( 'NONE',  ( 91.74479999999999791, -3644.899999999999636, 2261.869999999999891 ) ) ;
#8759 = CARTESIAN_POINT ( 'NONE',  ( 14.50925869426821713, -3657.309602984159483, 2247.678649714388030 ) ) ;
#8760 = CARTESIAN_POINT ( 'NONE',  ( 137.1599999999999397, -3694.509865589630408, 2255.773999999999432 ) ) ;
#8761 = AXIS2_PLACEMENT_3D ( 'NONE', #19667, #12518, #21774 ) ;
#8762 = CARTESIAN_POINT ( 'NONE',  ( 12.69999999999999929, -3659.504999999999654, 2245.359999999999673 ) ) ;
#8763 = EDGE_LOOP ( 'NONE', ( #13879, #18506, #17793, #16697 ) ) ;
#8764 = TOROIDAL_SURFACE ( 'NONE', #13023, 4.114799999999999791, 1.270000000000000018 ) ;
#8765 = CARTESIAN_POINT ( 'NONE',  ( -6.349999999999999645, -3694.938000000000102, 2253.487999999999829 ) ) ;
#8766 = CARTESIAN_POINT ( 'NONE',  ( 17.78000000000000114, -3599.497499999999945, 2296.591799999999694 ) ) ;
#8767 = CARTESIAN_POINT ( 'NONE',  ( 127.0000000000000000, -3568.700000000000273, 2261.869999999999891 ) ) ;
#8768 = DIRECTION ( 'NONE',  ( -1.000000000000000000, -0.000000000000000000, -0.000000000000000000 ) ) ;
#8769 = CARTESIAN_POINT ( 'NONE',  ( 10.36831320293767078, -3658.158799999985604, 2239.391000000000076 ) ) ;
#8770 = DIRECTION ( 'NONE',  ( 0.5000000000005969669, -0.8660254037840939834, 0.000000000000000000 ) ) ;
#8771 = APPLIED_DATE_AND_TIME_ASSIGNMENT ( #13603, #9961, ( #20503 ) ) ;
#8772 = CARTESIAN_POINT ( 'NONE',  ( 17.53979493689646674, -3576.455561739696350, 2245.871465501990315 ) ) ;
#8773 = DIRECTION ( 'NONE',  ( 0.000000000000000000, 0.000000000000000000, -1.000000000000000000 ) ) ;
#8774 = ORIENTED_EDGE ( 'NONE', *, *, #14188, .F. ) ;
#8775 = CARTESIAN_POINT ( 'NONE',  ( 0.7620000000000000107, -3694.938000000000102, 2275.001800000000003 ) ) ;
#8776 = EDGE_CURVE ( 'NONE', #14878, #7394, #14889, .T. ) ;
#8777 = DIRECTION ( 'NONE',  ( 0.8660254037820102058, 0.5000000000042060799, 0.000000000000000000 ) ) ;
#8778 = TOROIDAL_SURFACE ( 'NONE', #5031, 3.606799999998999695, 0.7620000000000000107 ) ;
#8779 = ORIENTED_EDGE ( 'NONE', *, *, #4777, .T. ) ;
#8780 = CARTESIAN_POINT ( 'NONE',  ( 38.10000000000000142, -3594.099999999999909, 2239.009999999999764 ) ) ;
#8781 = EDGE_CURVE ( 'NONE', #19866, #3918, #13012, .T. ) ;
#8782 = EDGE_LOOP ( 'NONE', ( #15550, #1757, #14406, #5887 ) ) ;
#8783 = CARTESIAN_POINT ( 'NONE',  ( 19.17699999999999960, -3579.494999999999891, 2239.771999999999935 ) ) ;
#8784 = ORIENTED_EDGE ( 'NONE', *, *, #9430, .T. ) ;
#8785 = ORIENTED_EDGE ( 'NONE', *, *, #3399, .F. ) ;
#8786 = ORIENTED_EDGE ( 'NONE', *, *, #21726, .F. ) ;
#8787 = CARTESIAN_POINT ( 'NONE',  ( 15.54479999999999862, -3579.494999999999891, 2256.063560000000052 ) ) ;
#8788 = ORIENTED_EDGE ( 'NONE', *, *, #8712, .F. ) ;
#8789 = CYLINDRICAL_SURFACE ( 'NONE', #17873, 5.460999999999938126 ) ;
#8790 = VECTOR ( 'NONE', #20994, 1000.000000000000000 ) ;
#8791 = SHAPE_DEFINITION_REPRESENTATION ( #19299, #3816 ) ;
#8792 = CIRCLE ( 'NONE', #6171, 3.606799999999001027 ) ;
#8793 = CARTESIAN_POINT ( 'NONE',  ( 22.54063073453000143, -3694.938000000000102, 2275.763800000000174 ) ) ;
#8794 = CARTESIAN_POINT ( 'NONE',  ( 15.52686321059681518, -3579.859966820806676, 2250.062296236718339 ) ) ;
#8795 = CYLINDRICAL_SURFACE ( 'NONE', #17879, 2.844799999999994444 ) ;
#8796 = APPLIED_PERSON_AND_ORGANIZATION_ASSIGNMENT ( #6518, #2986, ( #12762 ) ) ;
#8797 = CARTESIAN_POINT ( 'NONE',  ( 15.41268679713999923, -3641.068670452999868, 2296.591799999999694 ) ) ;
#8798 = DIRECTION ( 'NONE',  ( 1.000000000000000000, 0.000000000000000000, 0.000000000000000000 ) ) ;
#8799 = ORIENTED_EDGE ( 'NONE', *, *, #4555, .F. ) ;
#8800 = CARTESIAN_POINT ( 'NONE',  ( -12.31900000000000084, -3580.206200000000081, 2245.060313203000078 ) ) ;
#8801 = EDGE_CURVE ( 'NONE', #13188, #16556, #5528, .T. ) ;
#8802 = CARTESIAN_POINT ( 'NONE',  ( 15.07358448401000217, -3577.918427944000086, 2257.848701151000114 ) ) ;
#8803 = EDGE_LOOP ( 'NONE', ( #13339, #20852 ) ) ;
#8804 = TOROIDAL_SURFACE ( 'NONE', #1691, 3.606799999999999784, 0.7620000000000000107 ) ;
#8805 = CARTESIAN_POINT ( 'NONE',  ( 5.080000000000000071, -3694.430000000000291, 2260.600000000000364 ) ) ;
#8806 = DIRECTION ( 'NONE',  ( 0.000000000000000000, 0.000000000000000000, -1.000000000000000000 ) ) ;
#8807 = VECTOR ( 'NONE', #6564, 1000.000000000000000 ) ;
#8808 = EDGE_CURVE ( 'NONE', #12928, #17318, #20291, .T. ) ;
#8810 = EDGE_CURVE ( 'NONE', #13309, #5311, #16731, .T. ) ;
#8809 = VECTOR ( 'NONE', #8084, 1000.000000000000000 ) ;
#8811 = CARTESIAN_POINT ( 'NONE',  ( 15.24000000000000021, -3695.699999999999818, 2255.774000000000342 ) ) ;
#8812 = TOROIDAL_SURFACE ( 'NONE', #12171, 6.477000000000000313, 0.7620000000000000107 ) ;
#8813 = ORIENTED_EDGE ( 'NONE', *, *, #7813, .T. ) ;
#8814 = DIRECTION ( 'NONE',  ( 0.000000000000000000, 0.000000000000000000, -1.000000000000000000 ) ) ;
#8815 = CARTESIAN_POINT ( 'NONE',  ( 95.25000000000000000, -3670.300000000000182, 2244.547199999999975 ) ) ;
#8816 = ORIENTED_EDGE ( 'NONE', *, *, #19476, .F. ) ;
#8817 = DIRECTION ( 'NONE',  ( 0.000000000000000000, 0.000000000000000000, 1.000000000000000000 ) ) ;
#8818 = CARTESIAN_POINT ( 'NONE',  ( 9.285288183368999526, -3544.570000000000164, 2254.853250718999789 ) ) ;
#8819 = CARTESIAN_POINT ( 'NONE',  ( 12.70000000005999929, -3656.812599999999748, 2239.391000000000076 ) ) ;
#8820 = PERSON_AND_ORGANIZATION ( #5446, #1895 ) ;
#8821 = FACE_OUTER_BOUND ( 'NONE', #5798, .T. ) ;
#8822 = DIRECTION ( 'NONE',  ( 0.000000000000000000, 0.000000000000000000, -1.000000000000000000 ) ) ;
#8823 = DIRECTION ( 'NONE',  ( 0.000000000000000000, 0.000000000000000000, -1.000000000000000000 ) ) ;
#8824 = EDGE_CURVE ( 'NONE', #16556, #11901, #13477, .T. ) ;
#8825 = AXIS2_PLACEMENT_3D ( 'NONE', #3122, #15903, #22795 ) ;
#8826 = AXIS2_PLACEMENT_3D ( 'NONE', #9217, #9098, #12618 ) ;
#8827 = CARTESIAN_POINT ( 'NONE',  ( 137.0863986929037708, -3658.381654322079612, 2249.628458754722033 ) ) ;
#8828 = ORIENTED_EDGE ( 'NONE', *, *, #14605, .T. ) ;
#8829 = CARTESIAN_POINT ( 'NONE',  ( 137.0887894918462280, -3660.636540989195510, 2250.194016773457861 ) ) ;
#8830 = ORIENTED_EDGE ( 'NONE', *, *, #12662, .F. ) ;
#8831 = ORIENTED_EDGE ( 'NONE', *, *, #5991, .T. ) ;
#8832 = EDGE_LOOP ( 'NONE', ( #8870, #9969, #1215 ) ) ;
#8833 = ADVANCED_FACE ( 'NONE', ( #17108 ), #5896, .F. ) ;
#8834 = CARTESIAN_POINT ( 'NONE',  ( 0.000000000000000000, -3660.140000000000327, 2247.392000000000280 ) ) ;
#8835 = ORIENTED_EDGE ( 'NONE', *, *, #1353, .F. ) ;
#8836 = EDGE_LOOP ( 'NONE', ( #17558, #21613, #9241, #2715, #21486, #1305, #4589, #102 ) ) ;
#8837 = AXIS2_PLACEMENT_3D ( 'NONE', #3099, #21275, #14129 ) ;
#8838 = CARTESIAN_POINT ( 'NONE',  ( 12.69999999999999929, -3642.347301254450485, 2279.817638608977632 ) ) ;
#8839 = PERSON_AND_ORGANIZATION_ROLE ( 'classification_officer' ) ;
#8840 = DIRECTION ( 'NONE',  ( 1.000000000000000000, 0.000000000000000000, 0.000000000000000000 ) ) ;
#8841 = TOROIDAL_SURFACE ( 'NONE', #18550, 5.080000000000000071, 0.3810000000000000053 ) ;
#8842 = CARTESIAN_POINT ( 'NONE',  ( 3.175000000003000089, -3694.938000000000102, 2275.001800000000003 ) ) ;
#8843 = EDGE_CURVE ( 'NONE', #6254, #9478, #9267, .T. ) ;
#8844 = ORIENTED_EDGE ( 'NONE', *, *, #16996, .T. ) ;
#8845 = AXIS2_PLACEMENT_3D ( 'NONE', #10599, #17740, #4744 ) ;
#8846 = ADVANCED_FACE ( 'NONE', ( #9505 ), #15130, .T. ) ;
#8847 = DIRECTION ( 'NONE',  ( -1.000000000000000000, 0.000000000000000000, 0.000000000000000000 ) ) ;
#8848 = DIRECTION ( 'NONE',  ( -2.324635735433000053E-14, 2.336881798971000105E-14, -1.000000000000000000 ) ) ;
#8849 = FACE_OUTER_BOUND ( 'NONE', #1642, .T. ) ;
#8850 = PLANE ( 'NONE',  #17730 ) ;
#8851 = AXIS2_PLACEMENT_3D ( 'NONE', #6650, #20930, #4634 ) ;
#8852 = ORIENTED_EDGE ( 'NONE', *, *, #4131, .T. ) ;
#8853 = CALENDAR_DATE ( 2026, 26, 10 ) ;
#8854 = ORIENTED_EDGE ( 'NONE', *, *, #2856, .F. ) ;
#8855 = CIRCLE ( 'NONE', #17433, 3.175000000000149925 ) ;
#8856 = CARTESIAN_POINT ( 'NONE',  ( 7.238999999999998991, -3639.502500000000055, 2296.210799999999836 ) ) ;
#8857 = EDGE_CURVE ( 'NONE', #15808, #9634, #20179, .T. ) ;
#8858 = FACE_OUTER_BOUND ( 'NONE', #7253, .T. ) ;
#8859 = CARTESIAN_POINT ( 'NONE',  ( 50.79999999999999716, -3670.300000000000182, 2239.771999999999935 ) ) ;
#8860 = VERTEX_POINT ( 'NONE', #20510 ) ;
#8861 = ADVANCED_FACE ( 'NONE', ( #936 ), #11879, .T. ) ;
#8862 = CARTESIAN_POINT ( 'NONE',  ( 76.20000000000000284, -3568.700000000000273, 2259.837999999999738 ) ) ;
#8863 = CIRCLE ( 'NONE', #21949, 3.606799999999993567 ) ;
#8864 = CARTESIAN_POINT ( 'NONE',  ( 0.000000000000000000, -3695.699999999999818, 2275.001800000000003 ) ) ;
#8865 = CARTESIAN_POINT ( 'NONE',  ( 144.4983527463949713, -3576.390212577335205, 2245.979656122563938 ) ) ;
#8866 = DIRECTION ( 'NONE',  ( 1.000000000000000000, 0.000000000000000000, 0.000000000000000000 ) ) ;
#8867 = DIRECTION ( 'NONE',  ( 0.000000000000000000, 1.000000000000000000, 0.000000000000000000 ) ) ;
#8868 = DIRECTION ( 'NONE',  ( -1.125343061319999876E-12, 1.000000000000000000, 0.000000000000000000 ) ) ;
#8869 = AXIS2_PLACEMENT_3D ( 'NONE', #73, #12723, #17994 ) ;
#8870 = ORIENTED_EDGE ( 'NONE', *, *, #5118, .T. ) ;
#8871 = CARTESIAN_POINT ( 'NONE',  ( 1.270000000000000018, -3694.430000000000291, 2259.329999999999927 ) ) ;
#8872 = DIRECTION ( 'NONE',  ( 0.000000000000000000, 1.000000000000000000, 0.000000000000000000 ) ) ;
#8873 = APPLICATION_CONTEXT ( 'configuration controlled 3d designs of mechanical parts and assemblies' ) ;
#8874 = EDGE_CURVE ( 'NONE', #10888, #2635, #1131, .T. ) ;
#8875 = CARTESIAN_POINT ( 'NONE',  ( 20.62424768829000143, -3695.699999999999818, 2259.837999999999738 ) ) ;
#8876 = CARTESIAN_POINT ( 'NONE',  ( 14.81100937555136987, -3657.598029303296244, 2248.669232965897208 ) ) ;
#8877 = CARTESIAN_POINT ( 'NONE',  ( 136.7382561681559991, -3695.684722677371155, 2254.718515783431940 ) ) ;
#8878 = VERTEX_POINT ( 'NONE', #2367 ) ;
#8879 = VECTOR ( 'NONE', #9026, 1000.000000000000000 ) ;
#8880 = LINE ( 'NONE', #7120, #3870 ) ;
#8881 = ORIENTED_EDGE ( 'NONE', *, *, #145, .T. ) ;
#8882 = VECTOR ( 'NONE', #8965, 1000.000000000000000 ) ;
#8883 = DIRECTION ( 'NONE',  ( 1.224646799147353207E-16, 1.000000000000000000, -0.000000000000000000 ) ) ;
#8884 = CARTESIAN_POINT ( 'NONE',  ( 101.5999999999999943, -3670.300000000000182, 2261.869999999999891 ) ) ;
#8885 = CALENDAR_DATE ( 2026, 26, 10 ) ;
#8886 = CARTESIAN_POINT ( 'NONE',  ( 53.64479999999999649, -3670.300000000000182, 2261.869999999999891 ) ) ;
#8887 = LINE ( 'NONE', #14279, #10862 ) ;
#8888 = DIRECTION ( 'NONE',  ( 1.000000000000000000, 0.000000000000000000, 0.000000000000000000 ) ) ;
#8889 = EDGE_CURVE ( 'NONE', #20430, #17962, #16648, .T. ) ;
#8890 = DIRECTION ( 'NONE',  ( 0.000000000000000000, 1.000000000000000000, 0.000000000000000000 ) ) ;
#8891 = EDGE_LOOP ( 'NONE', ( #19096, #1183 ) ) ;
#8892 = DIRECTION ( 'NONE',  ( 1.000000000000000000, 0.000000000000000000, 0.000000000000000000 ) ) ;
#8893 = VERTEX_POINT ( 'NONE', #6001 ) ;
#8894 = LINE ( 'NONE', #17437, #3196 ) ;
#8895 = AXIS2_PLACEMENT_3D ( 'NONE', #5777, #5657, #268 ) ;
#8896 = DIRECTION ( 'NONE',  ( -1.000000000000000000, 0.000000000000000000, 0.000000000000000000 ) ) ;
#8897 = ORIENTED_EDGE ( 'NONE', *, *, #13215, .T. ) ;
#8898 = CARTESIAN_POINT ( 'NONE',  ( 35.56000000000000227, -3568.700000000000273, 2250.236800000000130 ) ) ;
#8899 = CIRCLE ( 'NONE', #15257, 5.079999999999973426 ) ;
#8900 = VERTEX_POINT ( 'NONE', #16769 ) ;
#8901 = DIRECTION ( 'NONE',  ( 0.000000000000000000, 0.000000000000000000, -1.000000000000000000 ) ) ;
#8902 = CARTESIAN_POINT ( 'NONE',  ( 151.1299999999999955, -3578.860000000000127, 2247.392000000000280 ) ) ;
#8903 = EDGE_LOOP ( 'NONE', ( #18187, #11530 ) ) ;
#8904 = ORIENTED_EDGE ( 'NONE', *, *, #20380, .T. ) ;
#8905 = LINE ( 'NONE', #16617, #15103 ) ;
#8906 = ORIENTED_EDGE ( 'NONE', *, *, #10143, .T. ) ;
#8907 = CARTESIAN_POINT ( 'NONE',  ( 15.03168679710029743, -3658.158799999889197, 2239.391000000000076 ) ) ;
#8908 = COORDINATED_UNIVERSAL_TIME_OFFSET ( 0, 0, .AHEAD. ) ;
#8909 = DIRECTION ( 'NONE',  ( 0.000000000000000000, -1.000000000000000000, 0.000000000000000000 ) ) ;
#8910 = DIRECTION ( 'NONE',  ( -2.324635735433000053E-14, 2.336881798971000105E-14, -1.000000000000000000 ) ) ;
#8911 = LINE ( 'NONE', #12656, #15270 ) ;
#8912 = VECTOR ( 'NONE', #20432, 1000.000000000000000 ) ;
#8913 = CYLINDRICAL_SURFACE ( 'NONE', #3852, 0.3810000000000260956 ) ;
#8914 = DIRECTION ( 'NONE',  ( 1.000000000000000000, 0.000000000000000000, 0.000000000000000000 ) ) ;
#8915 = VERTEX_POINT ( 'NONE', #715 ) ;
#8916 = DIRECTION ( 'NONE',  ( 0.000000000000000000, -1.000000000000000000, 0.000000000000000000 ) ) ;
#8917 = CARTESIAN_POINT ( 'NONE',  ( 15.33662675678000120, -3578.414664496000114, 2257.909780506000061 ) ) ;
#8918 = EDGE_LOOP ( 'NONE', ( #21242, #20037 ) ) ;
#8919 = CARTESIAN_POINT ( 'NONE',  ( 4.769632180749402650, -3695.600514564973764, 2259.822746372431993 ) ) ;
#8920 = EDGE_LOOP ( 'NONE', ( #10008, #4774, #11414, #14672 ) ) ;
#8921 = CARTESIAN_POINT ( 'NONE',  ( 152.4000000000000057, -3695.699999999999818, 2275.001800000000003 ) ) ;
#8922 = CARTESIAN_POINT ( 'NONE',  ( 145.0128742528000032, -3657.399152860999493, 2246.630000000000109 ) ) ;
#8923 = ORIENTED_EDGE ( 'NONE', *, *, #20342, .F. ) ;
#8924 = DIRECTION ( 'NONE',  ( 0.8928571428588618630, -0.4503400076008236552, 0.000000000000000000 ) ) ;
#8925 = CARTESIAN_POINT ( 'NONE',  ( 19.05000000000000071, -3660.140000000000327, 2247.392000000000280 ) ) ;
#8926 = B_SPLINE_CURVE_WITH_KNOTS ( 'NONE', 3,
 ( #12551, #6501, #9037, #16183, #136, #1206, #14551, #2125, #9156, #2238, #20280, #7506, #10908, #21690, #19819, #12667, #21916, #3994, #19934 ),
 .UNSPECIFIED., .F., .F.,
 ( 4, 1, 1, 1, 1, 1, 1, 1, 1, 1, 1, 1, 1, 1, 1, 1, 4 ),
 ( 3.168591426078754222E-06, 0.06250000000000000000, 0.1250000000000000000, 0.1875000000000000000, 0.2500000000000000000, 0.3125000000000000000, 0.3750000000000000000, 0.4375000000000000000, 0.5000000000000000000, 0.5625000000000000000, 0.6250000000000000000, 0.6875000000000000000, 0.7500000000000000000, 0.8125000000000000000, 0.8750000000000000000, 0.9375000000000000000, 1.000000000000000000 ),
 .UNSPECIFIED. ) ;
#8927 = ORIENTED_EDGE ( 'NONE', *, *, #5999, .T. ) ;
#8928 = APPLIED_PERSON_AND_ORGANIZATION_ASSIGNMENT ( #963, #20897, ( #12365 ) ) ;
#8929 = CARTESIAN_POINT ( 'NONE',  ( 6.985000000000000320, -3639.502500000000055, 2288.971800000000258 ) ) ;
#8930 = CARTESIAN_POINT ( 'NONE',  ( 1.270000000000000018, -3694.430000000000291, 2239.009999999999764 ) ) ;
#8931 = SHAPE_REPRESENTATION_RELATIONSHIP ( 'NONE' , 'NONE' ,  #8615, #8513 ) ;
#8932 = ADVANCED_FACE ( 'NONE', ( #19341 ), #1283, .T. ) ;
#8933 = DIRECTION ( 'NONE',  ( 0.000000000000000000, -1.000000000000000000, 0.000000000000000000 ) ) ;
#8934 = DIRECTION ( 'NONE',  ( 0.000000000000000000, 0.000000000000000000, 1.000000000000000000 ) ) ;
#8935 = CALENDAR_DATE ( 2026, 26, 10 ) ;
#8936 = EDGE_CURVE ( 'NONE', #21490, #5839, #1818, .T. ) ;
#8937 = DIRECTION ( 'NONE',  ( -1.206520773835000154E-12, -1.000000000000000000, 2.336881798973999985E-14 ) ) ;
#8938 = CARTESIAN_POINT ( 'NONE',  ( 10.15999999990231650, -3694.746619022270806, 2255.773999999897569 ) ) ;
#8939 = ORIENTED_EDGE ( 'NONE', *, *, #9526, .F. ) ;
#8941 = EDGE_CURVE ( 'NONE', #7082, #16518, #10752, .T. ) ;
#8940 = FACE_OUTER_BOUND ( 'NONE', #18793, .T. ) ;
#8942 = EDGE_CURVE ( 'NONE', #5409, #19963, #17456, .T. ) ;
#8943 = DIRECTION ( 'NONE',  ( 1.000000000000000000, 0.000000000000000000, 0.000000000000000000 ) ) ;
#8944 = VERTEX_POINT ( 'NONE', #22728 ) ;
#8945 = AXIS2_PLACEMENT_3D ( 'NONE', #13102, #2772, #2443 ) ;
#8946 = DIRECTION ( 'NONE',  ( 0.000000000000000000, 0.000000000000000000, 1.000000000000000000 ) ) ;
#8947 = ORIENTED_EDGE ( 'NONE', *, *, #22587, .T. ) ;
#8948 = ADVANCED_FACE ( 'NONE', ( #3043 ), #4923, .T. ) ;
#8949 = ORIENTED_EDGE ( 'NONE', *, *, #5203, .F. ) ;
#8950 = ORIENTED_EDGE ( 'NONE', *, *, #8384, .F. ) ;
#8951 = FACE_OUTER_BOUND ( 'NONE', #13292, .T. ) ;
#8952 = VERTEX_POINT ( 'NONE', #5169 ) ;
#8953 = ORIENTED_EDGE ( 'NONE', *, *, #17655, .F. ) ;
#8954 = DIRECTION ( 'NONE',  ( 2.336881798971000105E-14, 0.000000000000000000, 1.000000000000000000 ) ) ;
#8955 = ADVANCED_FACE ( 'NONE', ( #6920 ), #13834, .T. ) ;
#8956 = CALENDAR_DATE ( 2026, 26, 10 ) ;
#8957 = FACE_OUTER_BOUND ( 'NONE', #1806, .T. ) ;
#8958 = CARTESIAN_POINT ( 'NONE',  ( 17.77999999999999758, -3639.502500000000055, 2290.241799999999785 ) ) ;
#8959 = AXIS2_PLACEMENT_3D ( 'NONE', #1821, #17393, #13899 ) ;
#8960 = ORIENTED_EDGE ( 'NONE', *, *, #16870, .F. ) ;
#8961 = CARTESIAN_POINT ( 'NONE',  ( 10.36831320285999958, -3580.841199999999844, 2239.391000000000076 ) ) ;
#8962 = FACE_BOUND ( 'NONE', #2729, .T. ) ;
#8963 = DIRECTION ( 'NONE',  ( 0.000000000000000000, -1.000000000000000000, 0.000000000000000000 ) ) ;
#8964 = CIRCLE ( 'NONE', #5598, 0.7619999999999294005 ) ;
#8965 = DIRECTION ( 'NONE',  ( 0.000000000000000000, 1.000000000000000000, 0.000000000000000000 ) ) ;
#8966 = PERSON_AND_ORGANIZATION_ROLE ( 'creator' ) ;
#8967 = VERTEX_POINT ( 'NONE', #1406 ) ;
#8968 = CARTESIAN_POINT ( 'NONE',  ( -12.31900000000001505, -3658.793799999857129, 2249.723686796825405 ) ) ;
#8969 = EDGE_CURVE ( 'NONE', #22318, #4269, #20825, .T. ) ;
#8970 = DIRECTION ( 'NONE',  ( -1.000000000000000000, 0.000000000000000000, 0.000000000000000000 ) ) ;
#8971 = ORIENTED_EDGE ( 'NONE', *, *, #20722, .F. ) ;
#8972 = FACE_OUTER_BOUND ( 'NONE', #11772, .T. ) ;
#8973 = CIRCLE ( 'NONE', #22054, 0.7619999999999294005 ) ;
#8974 = APPROVAL_PERSON_ORGANIZATION ( #12480, #4060, #21389 ) ;
#8975 = CARTESIAN_POINT ( 'NONE',  ( 144.3372440649679049, -3576.154474778157237, 2246.502950162860998 ) ) ;
#8976 = AXIS2_PLACEMENT_3D ( 'NONE', #9078, #21622, #5450 ) ;
#8977 = CARTESIAN_POINT ( 'NONE',  ( 139.6999999999999886, -3659.504999999999654, 2239.009999999999764 ) ) ;
#8978 = DIRECTION ( 'NONE',  ( -1.000000000000000000, 0.000000000000000000, 0.000000000000000000 ) ) ;
#8979 = CARTESIAN_POINT ( 'NONE',  ( 18.24452305891707127, -3658.119603952914076, 2245.389097658092851 ) ) ;
#8980 = ORIENTED_EDGE ( 'NONE', *, *, #10431, .T. ) ;
#8981 = CARTESIAN_POINT ( 'NONE',  ( 10.36831320285999958, -3658.158799999999701, 2242.820000000000164 ) ) ;
#8982 = DIRECTION ( 'NONE',  ( -1.000000000000000000, 0.000000000000000000, 0.000000000000000000 ) ) ;
#8983 = FACE_OUTER_BOUND ( 'NONE', #15986, .T. ) ;
#8984 = CARTESIAN_POINT ( 'NONE',  ( 14.50229919307735571, -3657.303941002375723, 2247.615651459047967 ) ) ;
#8985 = PLANE ( 'NONE',  #20309 ) ;
#8986 = ORIENTED_EDGE ( 'NONE', *, *, #10558, .F. ) ;
#8987 = CARTESIAN_POINT ( 'NONE',  ( 64.76999999999999602, -3694.938000000000102, 2292.819899999999961 ) ) ;
#8988 = EDGE_LOOP ( 'NONE', ( #6689, #20652, #11565, #20387, #481, #13898 ) ) ;
#8989 = AXIS2_PLACEMENT_3D ( 'NONE', #212, #3951, #14742 ) ;
#8990 = CARTESIAN_POINT ( 'NONE',  ( 1.270000000000000018, -3660.140000000000327, 2247.392000000000280 ) ) ;
#8991 = APPLIED_APPROVAL_ASSIGNMENT ( #6342, ( #1759 ) ) ;
#8992 = AXIS2_PLACEMENT_3D ( 'NONE', #1280, #11712, #4803 ) ;
#8993 = FACE_OUTER_BOUND ( 'NONE', #20728, .T. ) ;
#8994 = CALENDAR_DATE ( 2026, 26, 10 ) ;
#8995 = DIRECTION ( 'NONE',  ( 0.8660254037825501072, 0.5000000000032710501, 0.000000000000000000 ) ) ;
#8996 = CARTESIAN_POINT ( 'NONE',  ( 104.4447999999999865, -3619.500000000000000, 2239.771999999999935 ) ) ;
#8997 = FACE_OUTER_BOUND ( 'NONE', #8318, .T. ) ;
#8998 = DIRECTION ( 'NONE',  ( 0.000000000000000000, 0.000000000000000000, -1.000000000000000000 ) ) ;
#8999 = EDGE_CURVE ( 'NONE', #20116, #15997, #16002, .T. ) ;
#9000 = EDGE_CURVE ( 'NONE', #8155, #22365, #10529, .T. ) ;
#9001 = ADVANCED_FACE ( 'NONE', ( #10891 ), #8789, .T. ) ;
#9002 = ORIENTED_EDGE ( 'NONE', *, *, #12510, .T. ) ;
#9003 = DIRECTION ( 'NONE',  ( 0.000000000000000000, 1.000000000000000000, 0.000000000000000000 ) ) ;
#9004 = VERTEX_POINT ( 'NONE', #16053 ) ;
#9005 = CIRCLE ( 'NONE', #5259, 0.7619999999999294005 ) ;
#9006 = FACE_OUTER_BOUND ( 'NONE', #16609, .T. ) ;
#9007 = DIRECTION ( 'NONE',  ( 0.000000000000000000, -1.000000000000000000, 0.000000000000000000 ) ) ;
#9008 = ORIENTED_EDGE ( 'NONE', *, *, #2624, .F. ) ;
#9009 = APPLIED_SECURITY_CLASSIFICATION_ASSIGNMENT ( #2620, ( #23167 ) ) ;
#9010 = EDGE_CURVE ( 'NONE', #13782, #185, #672, .T. ) ;
#9011 = DIRECTION ( 'NONE',  ( -1.000000000000000000, 0.000000000000000000, 0.000000000000000000 ) ) ;
#9012 = LOCAL_TIME ( 17, 37, 43.00000000000000000, #544 ) ;
#9013 = TOROIDAL_SURFACE ( 'NONE', #16858, 1.905000000000000027, 1.270000000000000018 ) ;
#9014 = ORIENTED_EDGE ( 'NONE', *, *, #10451, .F. ) ;
#9015 = FACE_BOUND ( 'NONE', #17374, .T. ) ;
#9016 = DIRECTION ( 'NONE',  ( 1.000000000000000000, 5.432398939370942693E-28, -2.324635735433000053E-14 ) ) ;
#9017 = ADVANCED_FACE ( 'NONE', ( #14648 ), #19569, .F. ) ;
#9018 = EDGE_LOOP ( 'NONE', ( #22276, #14657, #10704, #1788 ) ) ;
#9019 = ADVANCED_FACE ( 'NONE', ( #9141 ), #18040, .T. ) ;
#9020 = CARTESIAN_POINT ( 'NONE',  ( 137.7360682368147877, -3581.553478357457152, 2248.308632888655666 ) ) ;
#9021 = EDGE_LOOP ( 'NONE', ( #14223, #13741 ) ) ;
#9022 = CARTESIAN_POINT ( 'NONE',  ( 95.25000000000000000, -3543.299999999999727, 2247.392000000000280 ) ) ;
#9023 = APPROVAL_STATUS ( 'not_yet_approved' ) ;
#9024 = CARTESIAN_POINT ( 'NONE',  ( 95.25000000000000000, -3695.699999999999818, 2247.392000000000280 ) ) ;
#9025 = ORGANIZATION ( 'NAUO-ORG8', 'UNSPECIFIED', 'UNSPECIFIED' ) ;
#9026 = DIRECTION ( 'NONE',  ( 0.000000000000000000, 0.000000000000000000, 1.000000000000000000 ) ) ;
#9027 = APPROVAL_PERSON_ORGANIZATION ( #2957, #21811, #10338 ) ;
#9028 = CARTESIAN_POINT ( 'NONE',  ( 15.03168679710029743, -3578.148799999889434, 2239.391000000000076 ) ) ;
#9029 = DIRECTION ( 'NONE',  ( -1.000000000000000000, 2.760304743598999993E-14, 0.000000000000000000 ) ) ;
#9030 = CARTESIAN_POINT ( 'NONE',  ( 139.4317159485291029, -3576.659585059088386, 2249.195327489805550 ) ) ;
#9031 = ORIENTED_EDGE ( 'NONE', *, *, #18248, .T. ) ;
#9032 = TOROIDAL_SURFACE ( 'NONE', #22117, 4.114799999999999791, 1.270000000000000018 ) ;
#9033 = CARTESIAN_POINT ( 'NONE',  ( 134.0531819916954248, -3578.609843495611130, 2244.556611876764237 ) ) ;
#9034 = ORIENTED_EDGE ( 'NONE', *, *, #15973, .F. ) ;
#9035 = CARTESIAN_POINT ( 'NONE',  ( 15.53593155406000115, -3579.219969270000092, 2257.960590233999937 ) ) ;
#9036 = ORIENTED_EDGE ( 'NONE', *, *, #17741, .T. ) ;
#9037 = CARTESIAN_POINT ( 'NONE',  ( 9.864080040025308804, -3579.770148078739112, 2257.960588549625299 ) ) ;
#9038 = CARTESIAN_POINT ( 'NONE',  ( 20.09942059832000183, -3544.570000000000164, 2260.390449568000349 ) ) ;
#9039 = ORIENTED_EDGE ( 'NONE', *, *, #6805, .T. ) ;
#9040 = LINE ( 'NONE', #7620, #9049 ) ;
#9041 = DIRECTION ( 'NONE',  ( 0.000000000000000000, 0.000000000000000000, -1.000000000000000000 ) ) ;
#9042 = ORIENTED_EDGE ( 'NONE', *, *, #5752, .F. ) ;
#9043 = DIRECTION ( 'NONE',  ( 0.000000000000000000, -2.336881798971000105E-14, -1.000000000000000000 ) ) ;
#9044 = CARTESIAN_POINT ( 'NONE',  ( 11.18998458582999866, -3641.920631437999873, 2279.715722610000284 ) ) ;
#9045 = DIRECTION ( 'NONE',  ( -1.000000000000000000, 0.000000000000000000, 0.000000000000000000 ) ) ;
#9047 = CARTESIAN_POINT ( 'NONE',  ( 123.3932000000010021, -3619.500000000000000, 2239.771999999999935 ) ) ;
#9046 = TOROIDAL_SURFACE ( 'NONE', #7923, 4.114799999999999791, 1.270000000000000018 ) ;
#9048 = COORDINATED_UNIVERSAL_TIME_OFFSET ( 0, 0, .AHEAD. ) ;
#9049 = VECTOR ( 'NONE', #9159, 1000.000000000000114 ) ;
#9050 = CARTESIAN_POINT ( 'NONE',  ( 1.270000000000000018, -3660.140000000000327, 2244.547199999999975 ) ) ;
#9051 = DIRECTION ( 'NONE',  ( 0.000000000000000000, 0.000000000000000000, -1.000000000000000000 ) ) ;
#9052 = ORIENTED_EDGE ( 'NONE', *, *, #19102, .T. ) ;
#9053 = CARTESIAN_POINT ( 'NONE',  ( -12.31900000000000084, -3660.140000000000327, 2244.679313203000220 ) ) ;
#9054 = CARTESIAN_POINT ( 'NONE',  ( 137.7383617481069109, -3657.443753316391849, 2248.304914619292504 ) ) ;
#9055 = ORIENTED_EDGE ( 'NONE', *, *, #5752, .T. ) ;
#9056 = CARTESIAN_POINT ( 'NONE',  ( 137.5318703103976077, -3661.346907438663948, 2249.968155576829304 ) ) ;
#9057 = APPLIED_PERSON_AND_ORGANIZATION_ASSIGNMENT ( #1633, #15823, ( #8248 ) ) ;
#9058 = ORIENTED_EDGE ( 'NONE', *, *, #19140, .F. ) ;
#9059 = VERTEX_POINT ( 'NONE', #21674 ) ;
#9060 = ORIENTED_EDGE ( 'NONE', *, *, #2416, .T. ) ;
#9061 = AXIS2_PLACEMENT_3D ( 'NONE', #21898, #5864, #13002 ) ;
#9062 = ORIENTED_EDGE ( 'NONE', *, *, #9935, .T. ) ;
#9063 = AXIS2_PLACEMENT_3D ( 'NONE', #5726, #14741, #19898 ) ;
#9064 = AXIS2_PLACEMENT_3D ( 'NONE', #14184, #19914, #5267 ) ;
#9065 = CYLINDRICAL_SURFACE ( 'NONE', #3597, 0.3809999999999121312 ) ;
#9066 = EDGE_CURVE ( 'NONE', #22364, #15258, #7760, .T. ) ;
#9067 = ORIENTED_EDGE ( 'NONE', *, *, #13323, .F. ) ;
#9068 = VERTEX_POINT ( 'NONE', #7046 ) ;
#9069 = B_SPLINE_CURVE_WITH_KNOTS ( 'NONE', 3,
 ( #6974, #3441, #8374, #12351 ),
 .UNSPECIFIED., .F., .F.,
 ( 4, 4 ),
 ( 0.000000000000000000, 1.000000000000000000 ),
 .UNSPECIFIED. ) ;
#9070 = CARTESIAN_POINT ( 'NONE',  ( 12.69999999999999929, -3659.504999999999654, 2244.978999999999814 ) ) ;
#9071 = EDGE_CURVE ( 'NONE', #19732, #10096, #19918, .T. ) ;
#9072 = CALENDAR_DATE ( 2026, 26, 10 ) ;
#9073 = DIRECTION ( 'NONE',  ( 0.000000000000000000, 0.000000000000000000, 1.000000000000000000 ) ) ;
#9074 = CARTESIAN_POINT ( 'NONE',  ( 139.6999999999999886, -3659.504999999999654, 2246.630000000000109 ) ) ;
#9075 = ADVANCED_FACE ( 'NONE', ( #7382 ), #21564, .T. ) ;
#9076 = ORIENTED_EDGE ( 'NONE', *, *, #7421, .F. ) ;
#9077 = DIRECTION ( 'NONE',  ( 1.000000000000000000, 0.000000000000000000, 0.000000000000000000 ) ) ;
#9078 = CARTESIAN_POINT ( 'NONE',  ( 12.69999999999999929, -3579.494999999999891, 2239.009999999999764 ) ) ;
#9079 = FACE_OUTER_BOUND ( 'NONE', #2296, .T. ) ;
#9080 = LINE ( 'NONE', #20095, #2502 ) ;
#9081 = AXIS2_PLACEMENT_3D ( 'NONE', #5951, #11320, #11543 ) ;
#9082 = APPROVAL_STATUS ( 'not_yet_approved' ) ;
#9083 = VERTEX_POINT ( 'NONE', #5629 ) ;
#9084 = CARTESIAN_POINT ( 'NONE',  ( 29.00679999999900005, -3670.300000000000182, 2239.009999999999764 ) ) ;
#9085 = EDGE_LOOP ( 'NONE', ( #19917, #15981 ) ) ;
#9086 = CIRCLE ( 'NONE', #5339, 2.844800000000001550 ) ;
#9087 = CIRCLE ( 'NONE', #16206, 0.3809999999999647002 ) ;
#9088 = AXIS2_PLACEMENT_3D ( 'NONE', #1478, #2775, #3009 ) ;
#9089 = DIRECTION ( 'NONE',  ( 0.000000000000000000, 0.000000000000000000, -1.000000000000000000 ) ) ;
#9090 = DIRECTION ( 'NONE',  ( 1.000000000000000000, 0.000000000000000000, 0.000000000000000000 ) ) ;
#9091 = EDGE_LOOP ( 'NONE', ( #11659, #12428, #19516, #16525 ) ) ;
#9092 = DIRECTION ( 'NONE',  ( -1.000000000000000000, -0.000000000000000000, -0.000000000000000000 ) ) ;
#9093 = DIRECTION ( 'NONE',  ( -1.000000000000000000, 0.000000000000000000, 0.000000000000000000 ) ) ;
#9094 = ADVANCED_BREP_SHAPE_REPRESENTATION ( '', ( #6209, #5611 ), #11980 ) ;
#9095 = FACE_OUTER_BOUND ( 'NONE', #18518, .T. ) ;
#9096 = CIRCLE ( 'NONE', #476, 0.7619999999999758078 ) ;
#9097 = DIRECTION ( 'NONE',  ( 0.000000000000000000, 0.000000000000000000, -1.000000000000000000 ) ) ;
#9098 = DIRECTION ( 'NONE',  ( 0.000000000000000000, 0.000000000000000000, -1.000000000000000000 ) ) ;
#9099 = EDGE_CURVE ( 'NONE', #15748, #7197, #284, .T. ) ;
#9100 = ORIENTED_EDGE ( 'NONE', *, *, #1850, .F. ) ;
#9101 = FACE_OUTER_BOUND ( 'NONE', #13166, .T. ) ;
#9102 = PLANE ( 'NONE',  #11752 ) ;
#9103 = TOROIDAL_SURFACE ( 'NONE', #19184, 3.606799999998999695, 0.7620000000000000107 ) ;
#9104 = EDGE_CURVE ( 'NONE', #2862, #15378, #5153, .T. ) ;
#9105 = CARTESIAN_POINT ( 'NONE',  ( 15.03168679717383682, -3660.851200000147401, 2239.167815367321055 ) ) ;
#9106 = EDGE_CURVE ( 'NONE', #10186, #20939, #21243, .T. ) ;
#9107 = TOROIDAL_SURFACE ( 'NONE', #11331, 5.080000000000000071, 0.3810000000000000053 ) ;
#9108 = CYLINDRICAL_SURFACE ( 'NONE', #10834, 2.844800000000091700 ) ;
#9109 = CARTESIAN_POINT ( 'NONE',  ( 142.6617438336326131, -3543.315277321872600, 2254.718515779005429 ) ) ;
#9110 = CARTESIAN_POINT ( 'NONE',  ( 137.0453000019917056, -3695.234698871024193, 2255.486749946129748 ) ) ;
#9111 = ORIENTED_EDGE ( 'NONE', *, *, #8005, .F. ) ;
#9112 = CARTESIAN_POINT ( 'NONE',  ( 7.817606081005259000, -3576.524523609905373, 2245.767529109110455 ) ) ;
#9113 = EDGE_LOOP ( 'NONE', ( #6536, #22727 ) ) ;
#9114 = CALENDAR_DATE ( 2026, 26, 10 ) ;
#9115 = CARTESIAN_POINT ( 'NONE',  ( 1.270000000000000018, -3578.860000000000127, 2250.236800000000130 ) ) ;
#9117 = CIRCLE ( 'NONE', #21089, 0.7620000000000000107 ) ;
#9116 = COORDINATED_UNIVERSAL_TIME_OFFSET ( 0, 0, .AHEAD. ) ;
#9118 = FACE_OUTER_BOUND ( 'NONE', #2905, .T. ) ;
#9119 = CARTESIAN_POINT ( 'NONE',  ( 105.2067999999999870, -3619.500000000000000, 2239.771999999999935 ) ) ;
#9120 = DIRECTION ( 'NONE',  ( -1.000000000000000000, 0.000000000000000000, 0.000000000000000000 ) ) ;
#9121 = AXIS2_PLACEMENT_3D ( 'NONE', #60, #1812, #21504 ) ;
#9122 = DIRECTION ( 'NONE',  ( -1.224646799147353207E-16, 1.000000000000000000, 0.000000000000000000 ) ) ;
#9123 = AXIS2_PLACEMENT_3D ( 'NONE', #3408, #10562, #1064 ) ;
#9124 = EDGE_LOOP ( 'NONE', ( #14182, #19654, #19039, #15489 ) ) ;
#9125 = FACE_OUTER_BOUND ( 'NONE', #1778, .T. ) ;
#9126 = ORIENTED_EDGE ( 'NONE', *, *, #15898, .T. ) ;
#9127 = CARTESIAN_POINT ( 'NONE',  ( 47.19319999999999737, -3568.700000000000273, 2239.009999999999764 ) ) ;
#9128 = CARTESIAN_POINT ( 'NONE',  ( 10.46794630892000022, -3637.728865433999999, 2279.591814147000150 ) ) ;
#9129 = ORIENTED_EDGE ( 'NONE', *, *, #15293, .T. ) ;
#9130 = CYLINDRICAL_SURFACE ( 'NONE', #3546, 2.844800000000001550 ) ;
#9131 = CIRCLE ( 'NONE', #14739, 0.7619999999999987894 ) ;
#9132 = ADVANCED_FACE ( 'NONE', ( #1990 ), #19758, .T. ) ;
#9133 = ORIENTED_EDGE ( 'NONE', *, *, #4910, .F. ) ;
#9134 = CARTESIAN_POINT ( 'NONE',  ( 142.4684590622430846, -3695.492037865699785, 2255.201583320599184 ) ) ;
#9135 = CARTESIAN_POINT ( 'NONE',  ( 142.5447969220999767, -3659.505006299999877, 2250.165025787000104 ) ) ;
#9136 = EDGE_LOOP ( 'NONE', ( #18905, #17968, #2625, #2366, #18310, #12183 ) ) ;
#9137 = EDGE_CURVE ( 'NONE', #9389, #19621, #17454, .T. ) ;
#9138 = EDGE_CURVE ( 'NONE', #3812, #14108, #5866, .T. ) ;
#9139 = CARTESIAN_POINT ( 'NONE',  ( 137.9028742141985049, -3581.700239090842388, 2247.226065275468045 ) ) ;
#9140 = ORIENTED_EDGE ( 'NONE', *, *, #10788, .F. ) ;
#9141 = FACE_OUTER_BOUND ( 'NONE', #6519, .T. ) ;
#9142 = DIRECTION ( 'NONE',  ( 0.000000000000000000, 0.000000000000000000, -1.000000000000000000 ) ) ;
#9143 = CARTESIAN_POINT ( 'NONE',  ( 35.56000000000000227, -3694.430000000000291, 2247.392000000000280 ) ) ;
#9144 = EDGE_CURVE ( 'NONE', #13263, #1742, #19007, .T. ) ;
#9145 = CIRCLE ( 'NONE', #10252, 11.11250000000000071 ) ;
#9146 = FACE_OUTER_BOUND ( 'NONE', #14252, .T. ) ;
#9147 = DIRECTION ( 'NONE',  ( -1.000000000000000000, 0.000000000000000000, 0.000000000000000000 ) ) ;
#9148 = CIRCLE ( 'NONE', #22980, 5.460999999999938126 ) ;
#9149 = CARTESIAN_POINT ( 'NONE',  ( 138.2611185054702787, -3577.039135743023053, 2249.578612792418426 ) ) ;
#9150 = ORIENTED_EDGE ( 'NONE', *, *, #10357, .T. ) ;
#9151 = CARTESIAN_POINT ( 'NONE',  ( 134.8157984830815224, -3576.527304683796956, 2245.762539383495550 ) ) ;
#9152 = EDGE_CURVE ( 'NONE', #15597, #9475, #7406, .T. ) ;
#9153 = ADVANCED_FACE ( 'NONE', ( #13110 ), #18382, .T. ) ;
#9154 = CARTESIAN_POINT ( 'NONE',  ( 127.0000000000000000, -3670.300000000000182, 2239.009999999999764 ) ) ;
#9155 = VERTEX_POINT ( 'NONE', #2451 ) ;
#9156 = CARTESIAN_POINT ( 'NONE',  ( 10.49449033964999956, -3581.299265058999936, 2257.813191440000082 ) ) ;
#9157 = DIRECTION ( 'NONE',  ( 0.8660254037817188832, -0.5000000000047110094, -1.484475890921031808E-12 ) ) ;
#9158 = ORIENTED_EDGE ( 'NONE', *, *, #3478, .T. ) ;
#9159 = DIRECTION ( 'NONE',  ( 0.8660254037842058938, 0.5000000000004030110, -5.443078266503040078E-12 ) ) ;
#9160 = DIRECTION ( 'NONE',  ( -1.000000000000000000, 0.000000000000000000, 0.000000000000000000 ) ) ;
#9161 = AXIS2_PLACEMENT_3D ( 'NONE', #8165, #11784, #18937 ) ;
#9162 = ORIENTED_EDGE ( 'NONE', *, *, #12641, .T. ) ;
#9163 = CARTESIAN_POINT ( 'NONE',  ( 10.36831320292846925, -3580.841200000038953, 2239.391000000000076 ) ) ;
#9164 = ADVANCED_FACE ( 'NONE', ( #574 ), #11130, .F. ) ;
#9165 = DIRECTION ( 'NONE',  ( 0.000000000000000000, 0.000000000000000000, -1.000000000000000000 ) ) ;
#9166 =( NAMED_UNIT ( * ) SI_UNIT ( $, .STERADIAN. ) SOLID_ANGLE_UNIT ( ) );
#9167 = VECTOR ( 'NONE', #5445, 1000.000000000000000 ) ;
#9168 = FACE_OUTER_BOUND ( 'NONE', #5571, .T. ) ;
#9169 = DIRECTION ( 'NONE',  ( -2.324635735433000053E-14, 2.336881798971000105E-14, -1.000000000000000000 ) ) ;
#9170 = COORDINATED_UNIVERSAL_TIME_OFFSET ( 0, 0, .AHEAD. ) ;
#9171 = ORIENTED_EDGE ( 'NONE', *, *, #9789, .T. ) ;
#9172 = CARTESIAN_POINT ( 'NONE',  ( 20.62424768829000143, -3694.430000000000291, 2260.600000000000364 ) ) ;
#9173 = CARTESIAN_POINT ( 'NONE',  ( 9.849683474922617421, -3695.600514565444882, 2254.996725890482594 ) ) ;
#9174 = ORIENTED_EDGE ( 'NONE', *, *, #19700, .F. ) ;
#9175 = CARTESIAN_POINT ( 'NONE',  ( 18.12475792849799205, -3581.293143188160229, 2245.917988635005713 ) ) ;
#9176 = LINE ( 'NONE', #16321, #18437 ) ;
#9177 = ORIENTED_EDGE ( 'NONE', *, *, #14885, .T. ) ;
#9178 = AXIS2_PLACEMENT_3D ( 'NONE', #5792, #19736, #5440 ) ;
#9179 = ORIENTED_EDGE ( 'NONE', *, *, #10946, .T. ) ;
#9180 = CARTESIAN_POINT ( 'NONE',  ( 141.7787351652112591, -3661.447272802506632, 2249.918713514176034 ) ) ;
#9181 = EDGE_CURVE ( 'NONE', #18205, #10888, #20264, .T. ) ;
#9182 = VECTOR ( 'NONE', #20248, 1000.000000000000000 ) ;
#9183 = AXIS2_PLACEMENT_3D ( 'NONE', #22053, #14811, #20637 ) ;
#9184 = EDGE_LOOP ( 'NONE', ( #19283, #9031, #10177, #13830 ) ) ;
#9185 = ORIENTED_EDGE ( 'NONE', *, *, #1329, .F. ) ;
#9186 = DIRECTION ( 'NONE',  ( 0.000000000000000000, 0.000000000000000000, -1.000000000000000000 ) ) ;
#9187 = ORIENTED_EDGE ( 'NONE', *, *, #23021, .F. ) ;
#9188 = ORIENTED_EDGE ( 'NONE', *, *, #5815, .F. ) ;
#9189 = DIRECTION ( 'NONE',  ( -0.000000000000000000, -1.000000000000000000, -0.000000000000000000 ) ) ;
#9190 = DIRECTION ( 'NONE',  ( 1.000000000000000000, 0.000000000000000000, 0.000000000000000000 ) ) ;
#9191 = VERTEX_POINT ( 'NONE', #20368 ) ;
#9192 = DIRECTION ( 'NONE',  ( 0.000000000000000000, 0.000000000000000000, 1.000000000000000000 ) ) ;
#9193 = CARTESIAN_POINT ( 'NONE',  ( -6.349999999999999645, -3660.140000000000327, 2247.392000000000280 ) ) ;
#9194 = CARTESIAN_POINT ( 'NONE',  ( 7.298181435199534661, -3581.361247027800346, 2246.035952059512510 ) ) ;
#9195 = AXIS2_PLACEMENT_3D ( 'NONE', #4251, #13490, #18540 ) ;
#9196 = AXIS2_PLACEMENT_3D ( 'NONE', #15807, #17792, #3264 ) ;
#9197 = DIRECTION ( 'NONE',  ( -0.000000000000000000, 1.000000000000000000, 0.000000000000000000 ) ) ;
#9198 = DATE_AND_TIME ( #14131, #6036 ) ;
#9199 = APPLIED_PERSON_AND_ORGANIZATION_ASSIGNMENT ( #16373, #12239, ( #10136 ) ) ;
#9200 = ORIENTED_EDGE ( 'NONE', *, *, #1463, .T. ) ;
#9201 = AXIS2_PLACEMENT_3D ( 'NONE', #19298, #3237, #19061 ) ;
#9202 = FACE_OUTER_BOUND ( 'NONE', #9303, .T. ) ;
#9203 = ORIENTED_EDGE ( 'NONE', *, *, #19549, .T. ) ;
#9204 = DIRECTION ( 'NONE',  ( -1.000000000000000000, 0.000000000000000000, 0.000000000000000000 ) ) ;
#9205 = ORIENTED_EDGE ( 'NONE', *, *, #8942, .F. ) ;
#9206 = CARTESIAN_POINT ( 'NONE',  ( 12.69999999999999929, -3661.409999999999400, 2270.760000000000218 ) ) ;
#9207 = CARTESIAN_POINT ( 'NONE',  ( 15.54479999999999862, -3599.497499999999945, 2288.971800000000258 ) ) ;
#9208 = ORIENTED_EDGE ( 'NONE', *, *, #4639, .F. ) ;
#9209 = CARTESIAN_POINT ( 'NONE',  ( 117.9067999999989951, -3594.099999999999909, 2259.837999999999738 ) ) ;
#9210 = TOROIDAL_SURFACE ( 'NONE', #16317, 3.606799999999999784, 0.7620000000000000107 ) ;
#9211 = DIRECTION ( 'NONE',  ( 0.000000000000000000, 0.000000000000000000, 1.000000000000000000 ) ) ;
#9212 = PLANE ( 'NONE',  #635 ) ;
#9213 = AXIS2_PLACEMENT_3D ( 'NONE', #4421, #7824, #20358 ) ;
#9214 = CARTESIAN_POINT ( 'NONE',  ( 12.69999999999999929, -3579.494999999999891, 2270.760000000000218 ) ) ;
#9215 = PRODUCT_DEFINITION_SHAPE ( 'NONE', 'NONE',  #20962 ) ;
#9216 = ORIENTED_EDGE ( 'NONE', *, *, #16303, .T. ) ;
#9217 = CARTESIAN_POINT ( 'NONE',  ( 139.6999999999999886, -3579.494999999999891, 2239.771999999999935 ) ) ;
#9218 = ORIENTED_EDGE ( 'NONE', *, *, #12530, .T. ) ;
#9219 = CARTESIAN_POINT ( 'NONE',  ( 147.3450958631953256, -3694.826579461069286, 2260.537176449191975 ) ) ;
#9220 = DIRECTION ( 'NONE',  ( -1.804050561861959928E-14, 0.5000000000033889558, -0.8660254037824819395 ) ) ;
#9221 = CARTESIAN_POINT ( 'NONE',  ( 38.10000000000000142, -3644.899999999999636, 2239.771999999999935 ) ) ;
#9222 = CIRCLE ( 'NONE', #18559, 1.269999999999882334 ) ;
#9223 = CARTESIAN_POINT ( 'NONE',  ( 12.69999999999999929, -3599.497499999999945, 2295.829799999999977 ) ) ;
#9224 = CARTESIAN_POINT ( 'NONE',  ( 114.2999999999999972, -3644.899999999999636, 2239.771999999999935 ) ) ;
#9225 = CARTESIAN_POINT ( 'NONE',  ( 137.0970213875862385, -3695.048176949268964, 2255.616427087924876 ) ) ;
#9226 = CARTESIAN_POINT ( 'NONE',  ( 7.481739961591920007, -3577.164555605966598, 2245.107626269509183 ) ) ;
#9227 = VERTEX_POINT ( 'NONE', #11570 ) ;
#9228 = PRODUCT_CONTEXT ( 'NONE', #11555, 'mechanical' ) ;
#9229 = APPLIED_PERSON_AND_ORGANIZATION_ASSIGNMENT ( #20009, #1959, ( #7499 ) ) ;
#9230 = FACE_OUTER_BOUND ( 'NONE', #9255, .T. ) ;
#9231 = CARTESIAN_POINT ( 'NONE',  ( 12.69999999999999929, -3579.494999999999891, 2270.760000000000218 ) ) ;
#9232 = APPROVAL_ROLE ( '' ) ;
#9233 = CARTESIAN_POINT ( 'NONE',  ( 12.69999999999999929, -3585.971999999999753, 2268.705139999999574 ) ) ;
#9234 = VECTOR ( 'NONE', #18507, 1000.000000000000000 ) ;
#9235 = EDGE_CURVE ( 'NONE', #21912, #15765, #10486, .T. ) ;
#9236 = DIRECTION ( 'NONE',  ( 0.000000000000000000, 0.000000000000000000, 1.000000000000000000 ) ) ;
#9237 = ADVANCED_FACE ( 'NONE', ( #12043 ), #3132, .T. ) ;
#9238 = CARTESIAN_POINT ( 'NONE',  ( 134.6064618253988101, -3662.097549161604093, 2245.303073078320722 ) ) ;
#9239 = EDGE_CURVE ( 'NONE', #22803, #17848, #17191, .T. ) ;
#9240 = VECTOR ( 'NONE', #8866, 1000.000000000000000 ) ;
#9241 = ORIENTED_EDGE ( 'NONE', *, *, #11296, .F. ) ;
#9242 = CARTESIAN_POINT ( 'NONE',  ( 88.90000000000000568, -3594.099999999999909, 2260.600000000000364 ) ) ;
#9243 = CARTESIAN_POINT ( 'NONE',  ( 12.59468037889999970, -3636.657701233000353, 2279.817639764999967 ) ) ;
#9244 = ORIENTED_EDGE ( 'NONE', *, *, #11432, .F. ) ;
#9245 = EDGE_CURVE ( 'NONE', #18657, #8438, #5488, .T. ) ;
#9246 = DIRECTION ( 'NONE',  ( 0.000000000000000000, 1.000000000000000000, 0.000000000000000000 ) ) ;
#9247 = EDGE_CURVE ( 'NONE', #8731, #21632, #16908, .T. ) ;
#9248 = AXIS2_PLACEMENT_3D ( 'NONE', #3659, #7300, #7988 ) ;
#9249 = AXIS2_PLACEMENT_3D ( 'NONE', #4950, #3071, #6953 ) ;
#9250 = ORIENTED_EDGE ( 'NONE', *, *, #10667, .T. ) ;
#9251 = CARTESIAN_POINT ( 'NONE',  ( 142.3391137066397221, -3695.185487565168842, 2255.525687528044273 ) ) ;
#9252 = DIRECTION ( 'NONE',  ( 0.000000000000000000, 0.000000000000000000, -1.000000000000000000 ) ) ;
#9253 = EDGE_CURVE ( 'NONE', #21213, #9634, #18620, .T. ) ;
#9254 = TOROIDAL_SURFACE ( 'NONE', #9970, 3.606799999999999784, 0.7620000000000000107 ) ;
#9255 = EDGE_LOOP ( 'NONE', ( #7857, #1319, #15370, #12041 ) ) ;
#9256 = AXIS2_PLACEMENT_3D ( 'NONE', #188, #7224, #4047 ) ;
#9257 = CARTESIAN_POINT ( 'NONE',  ( 137.2861954999169143, -3581.000367542877484, 2249.265958390819378 ) ) ;
#9258 = UNCERTAINTY_MEASURE_WITH_UNIT (LENGTH_MEASURE( 1.000000000000000082E-05 ), #17942, 'distance_accuracy_value', 'NONE');
#9259 = ORIENTED_EDGE ( 'NONE', *, *, #1942, .T. ) ;
#9260 = CARTESIAN_POINT ( 'NONE',  ( 123.3932000000010021, -3568.700000000000273, 2259.837999999999738 ) ) ;
#9261 = DATE_AND_TIME ( #5751, #7872 ) ;
#9262 = CARTESIAN_POINT ( 'NONE',  ( 114.2999999999999972, -3644.899999999999636, 2260.600000000000364 ) ) ;
#9263 = DIRECTION ( 'NONE',  ( 0.000000000000000000, 0.000000000000000000, 1.000000000000000000 ) ) ;
#9264 = CYLINDRICAL_SURFACE ( 'NONE', #19728, 0.3809999999999924558 ) ;
#9265 = EDGE_CURVE ( 'NONE', #14824, #20865, #13556, .T. ) ;
#9266 = CARTESIAN_POINT ( 'NONE',  ( 10.06337286646999907, -3578.414665316000082, 2257.909780569999839 ) ) ;
#9267 = CIRCLE ( 'NONE', #18995, 2.844800000000091700 ) ;
#9268 = CARTESIAN_POINT ( 'NONE',  ( 142.0937630362152788, -3577.955592839939072, 2250.090245135924306 ) ) ;
#9269 = ORIENTED_EDGE ( 'NONE', *, *, #14571, .F. ) ;
#9270 = CARTESIAN_POINT ( 'NONE',  ( -6.349999999999999645, -3660.140000000000327, 2250.998800000000301 ) ) ;
#9271 = EDGE_CURVE ( 'NONE', #18622, #13565, #5171, .T. ) ;
#9272 = CIRCLE ( 'NONE', #4759, 0.7619999999999294005 ) ;
#9273 = EDGE_CURVE ( 'NONE', #957, #17291, #7048, .T. ) ;
#9274 = TOROIDAL_SURFACE ( 'NONE', #11885, 6.477000000000000313, 0.7620000000000000107 ) ;
#9275 = CARTESIAN_POINT ( 'NONE',  ( 1.270000000000000018, -3578.860000000000127, 2247.392000000000280 ) ) ;
#9276 = ORIENTED_EDGE ( 'NONE', *, *, #12393, .T. ) ;
#9277 = CARTESIAN_POINT ( 'NONE',  ( 12.69999999996000106, -3642.194899999999961, 2292.781800000000203 ) ) ;
#9278 = LINE ( 'NONE', #2006, #8739 ) ;
#9279 = ORIENTED_EDGE ( 'NONE', *, *, #5704, .F. ) ;
#9280 = CARTESIAN_POINT ( 'NONE',  ( 4.572920519510000226, -3543.299999999999727, 2259.329999999999927 ) ) ;
#9281 = ORIENTED_EDGE ( 'NONE', *, *, #18736, .T. ) ;
#9282 = AXIS2_PLACEMENT_3D ( 'NONE', #11103, #4602, #2201 ) ;
#9283 = CARTESIAN_POINT ( 'NONE',  ( 12.69999999999999929, -3639.502500000000055, 2290.241799999999785 ) ) ;
#9284 = DIRECTION ( 'NONE',  ( 0.7249994335955246560, 0.000000000000000000, 0.6887494619135237084 ) ) ;
#9285 = SHAPE_REPRESENTATION_RELATIONSHIP ( 'NONE' , 'NONE' ,  #21348, #19727 ) ;
#9286 = DIRECTION ( 'NONE',  ( 0.000000000000000000, 0.000000000000000000, 1.000000000000000000 ) ) ;
#9287 = EDGE_LOOP ( 'NONE', ( #4423, #5335, #9667, #5666 ) ) ;
#9288 = DIRECTION ( 'NONE',  ( -0.000000000000000000, -1.000000000000000000, -0.000000000000000000 ) ) ;
#9289 = ADVANCED_FACE ( 'NONE', ( #12508 ), #19427, .F. ) ;
#9290 = APPLICATION_PROTOCOL_DEFINITION ( 'international standard', 'automotive_design', 2000, #16793 ) ;
#9291 = AXIS2_PLACEMENT_3D ( 'NONE', #5527, #125, #5283 ) ;
#9292 = CARTESIAN_POINT ( 'NONE',  ( 22.54063073453000143, -3543.299999999999727, 2275.763800000000174 ) ) ;
#9293 = CARTESIAN_POINT ( 'NONE',  ( 12.69999999999999929, -3659.504999999999654, 2246.630000000000109 ) ) ;
#9294 = ORIENTED_EDGE ( 'NONE', *, *, #12583, .T. ) ;
#9295 = CARTESIAN_POINT ( 'NONE',  ( 18.20689721057726373, -3581.023318642830418, 2245.544194210850492 ) ) ;
#9296 = CARTESIAN_POINT ( 'NONE',  ( 137.5404010602593985, -3657.652756290912748, 2248.773912801639653 ) ) ;
#9297 = EDGE_LOOP ( 'NONE', ( #1273, #10936 ) ) ;
#9298 = ORIENTED_EDGE ( 'NONE', *, *, #4227, .F. ) ;
#9299 = CARTESIAN_POINT ( 'NONE',  ( 137.2437110623308456, -3660.940235422853675, 2250.121982768094313 ) ) ;
#9300 = EDGE_CURVE ( 'NONE', #5448, #10412, #17898, .T. ) ;
#9301 = TOROIDAL_SURFACE ( 'NONE', #15653, 3.606799999998999695, 0.7620000000000000107 ) ;
#9302 = EDGE_CURVE ( 'NONE', #15238, #12083, #6292, .T. ) ;
#9303 = EDGE_LOOP ( 'NONE', ( #8939, #10715, #8506, #21210 ) ) ;
#9304 = EDGE_CURVE ( 'NONE', #14295, #21153, #12282, .T. ) ;
#9305 = ORIENTED_EDGE ( 'NONE', *, *, #12666, .F. ) ;
#9306 = CARTESIAN_POINT ( 'NONE',  ( 139.6999999999999886, -3579.494999999999891, 2246.630000000000109 ) ) ;
#9307 = ORIENTED_EDGE ( 'NONE', *, *, #16247, .T. ) ;
#9308 = VERTEX_POINT ( 'NONE', #18013 ) ;
#9309 = DIRECTION ( 'NONE',  ( 0.000000000000000000, -1.000000000000000000, 0.000000000000000000 ) ) ;
#9310 = DIRECTION ( 'NONE',  ( -0.7249994335945011414, 0.000000000000000000, 0.6887494619146010688 ) ) ;
#9311 = ADVANCED_FACE ( 'NONE', ( #19656 ), #10022, .T. ) ;
#9312 = VERTEX_POINT ( 'NONE', #18127 ) ;
#9313 = DIRECTION ( 'NONE',  ( 0.7249994335945011414, 6.337882393832011514E-14, -0.6887494619146010688 ) ) ;
#9314 = DIRECTION ( 'NONE',  ( 0.000000000000000000, 0.000000000000000000, 1.000000000000000000 ) ) ;
#9315 = EDGE_CURVE ( 'NONE', #12115, #12400, #2534, .T. ) ;
#9316 = APPROVAL_ROLE ( '' ) ;
#9317 = ADVANCED_FACE ( 'NONE', ( #8993 ), #12640, .T. ) ;
#9318 = CARTESIAN_POINT ( 'NONE',  ( 12.69999999999999929, -3649.471999999999753, 2261.593139999999948 ) ) ;
#9319 = AXIS2_PLACEMENT_3D ( 'NONE', #4083, #7829, #16952 ) ;
#9321 = CARTESIAN_POINT ( 'NONE',  ( 0.7620000000000000107, -3544.061999999999898, 2239.009999999999764 ) ) ;
#9320 = APPLICATION_CONTEXT ( 'configuration controlled 3d designs of mechanical parts and assemblies' ) ;
#9322 = CARTESIAN_POINT ( 'NONE',  ( 12.69999999999999929, -3584.956000000000131, 2245.359999999999673 ) ) ;
#9323 = B_SPLINE_CURVE_WITH_KNOTS ( 'NONE', 3,
 ( #10734, #14372, #10498, #21517 ),
 .UNSPECIFIED., .F., .F.,
 ( 4, 4 ),
 ( 0.000000000000000000, 1.000000000000000000 ),
 .UNSPECIFIED. ) ;
#9324 = DIRECTION ( 'NONE',  ( -2.324635735433000053E-14, 2.336881798971000105E-14, -1.000000000000000000 ) ) ;
#9325 = ORIENTED_EDGE ( 'NONE', *, *, #15164, .T. ) ;
#9326 = FACE_OUTER_BOUND ( 'NONE', #2381, .T. ) ;
#9327 = FACE_OUTER_BOUND ( 'NONE', #13169, .T. ) ;
#9328 = CARTESIAN_POINT ( 'NONE',  ( 15.03168679717000167, -3580.841199999999844, 2242.820000000000164 ) ) ;
#9329 = FACE_OUTER_BOUND ( 'NONE', #7299, .T. ) ;
#9330 = ORIENTED_EDGE ( 'NONE', *, *, #6816, .T. ) ;
#9331 = CARTESIAN_POINT ( 'NONE',  ( 18.12252087484897345, -3657.700112227995760, 2245.929179952064260 ) ) ;
#9332 = ORIENTED_EDGE ( 'NONE', *, *, #21318, .F. ) ;
#9333 = CARTESIAN_POINT ( 'NONE',  ( 12.69999999999999929, -3579.494999999999891, 2246.630000000000109 ) ) ;
#9334 = DIRECTION ( 'NONE',  ( 0.8660254037825932949, 0.5000000000031962211, 0.000000000000000000 ) ) ;
#9335 = VECTOR ( 'NONE', #9557, 1000.000000000000000 ) ;
#9336 = CARTESIAN_POINT ( 'NONE',  ( 1.270000000000000018, -3543.299999999999727, 2259.329999999999927 ) ) ;
#9337 = FACE_OUTER_BOUND ( 'NONE', #20168, .T. ) ;
#9338 = FACE_OUTER_BOUND ( 'NONE', #2935, .T. ) ;
#9339 = FACE_OUTER_BOUND ( 'NONE', #19313, .T. ) ;
#9340 = CARTESIAN_POINT ( 'NONE',  ( 7.562696255153550595, -3576.991455836282512, 2245.246524209903328 ) ) ;
#9341 = ORIENTED_EDGE ( 'NONE', *, *, #2065, .T. ) ;
#9342 = DATE_AND_TIME ( #10978, #20987 ) ;
#9343 = CARTESIAN_POINT ( 'NONE',  ( 21.79320000000099711, -3568.700000000000273, 2239.771999999999935 ) ) ;
#9344 = DIRECTION ( 'NONE',  ( -1.000000000000000000, 0.000000000000000000, 0.000000000000000000 ) ) ;
#9345 = CALENDAR_DATE ( 2026, 26, 10 ) ;
#9346 = VECTOR ( 'NONE', #6647, 1000.000000000000000 ) ;
#9347 = CARTESIAN_POINT ( 'NONE',  ( 151.1299999999999955, -3695.699999999999818, 2240.279999999999745 ) ) ;
#9348 = CARTESIAN_POINT ( 'NONE',  ( -12.31900000000000084, -3578.860000000000127, 2247.392000000000280 ) ) ;
#9349 =( GEOMETRIC_REPRESENTATION_CONTEXT ( 3 ) GLOBAL_UNCERTAINTY_ASSIGNED_CONTEXT ( ( #3532 ) ) GLOBAL_UNIT_ASSIGNED_CONTEXT ( ( #4715, #19130, #20642 ) ) REPRESENTATION_CONTEXT ( 'NONE', 'WORKASPACE' ) );
#9350 = CARTESIAN_POINT ( 'NONE',  ( 135.0627559351442244, -3662.845525222075139, 2246.502950163688183 ) ) ;
#9351 = ORIENTED_EDGE ( 'NONE', *, *, #14592, .F. ) ;
#9352 = DIRECTION ( 'NONE',  ( 0.000000000000000000, 0.000000000000000000, 1.000000000000000000 ) ) ;
#9353 = VERTEX_POINT ( 'NONE', #91 ) ;
#9354 = DIRECTION ( 'NONE',  ( -1.000000000000000000, 0.000000000000000000, 0.000000000000000000 ) ) ;
#9355 = APPLIED_DATE_AND_TIME_ASSIGNMENT ( #21011, #4951, ( #12365 ) ) ;
#9356 = FACE_OUTER_BOUND ( 'NONE', #854, .T. ) ;
#9357 = VERTEX_POINT ( 'NONE', #8766 ) ;
#9358 = CARTESIAN_POINT ( 'NONE',  ( 12.70000000005999929, -3656.812599999999748, 2242.820000000000164 ) ) ;
#9359 = CARTESIAN_POINT ( 'NONE',  ( 12.69999999999999929, -3579.494999999999891, 2272.030000000000200 ) ) ;
#9360 = EDGE_CURVE ( 'NONE', #22999, #14462, #14163, .T. ) ;
#9361 = VERTEX_POINT ( 'NONE', #17776 ) ;
#9362 = CARTESIAN_POINT ( 'NONE',  ( 142.5377065954122315, -3695.586719555400578, 2255.028323494163942 ) ) ;
#9363 = CARTESIAN_POINT ( 'NONE',  ( 12.69999999997567208, -3642.194900000083180, 2296.210799999999836 ) ) ;
#9364 = LOCAL_TIME ( 17, 37, 43.00000000000000000, #9624 ) ;
#9365 = EDGE_CURVE ( 'NONE', #452, #1809, #15913, .T. ) ;
#9366 = ORIENTED_EDGE ( 'NONE', *, *, #1, .F. ) ;
#9367 = ADVANCED_FACE ( 'NONE', ( #2085 ), #21307, .T. ) ;
#9368 = CARTESIAN_POINT ( 'NONE',  ( 137.8781067631969677, -3581.679898106256132, 2246.981755619571686 ) ) ;
#9369 = ORIENTED_EDGE ( 'NONE', *, *, #15029, .T. ) ;
#9370 = CARTESIAN_POINT ( 'NONE',  ( 145.3610525455973175, -3580.284312841534302, 2244.927052815919069 ) ) ;
#9371 = SECURITY_CLASSIFICATION_LEVEL ( 'unclassified' ) ;
#9372 = CARTESIAN_POINT ( 'NONE',  ( 18.41500000000100101, -3579.494999999999891, 2246.630000000000109 ) ) ;
#9373 = EDGE_CURVE ( 'NONE', #16752, #10141, #7467, .T. ) ;
#9374 = DIRECTION ( 'NONE',  ( 1.206643234470999950E-12, -1.000000000000000000, -2.336881798973999985E-14 ) ) ;
#9375 = CARTESIAN_POINT ( 'NONE',  ( 50.79999999999999716, -3568.700000000000273, 2239.771999999999935 ) ) ;
#9376 = CARTESIAN_POINT ( 'NONE',  ( 145.4149999978999972, -3659.505243078000149, 2244.618209833000492 ) ) ;
#9377 = APPROVAL_PERSON_ORGANIZATION ( #7047, #11201, #14192 ) ;
#9378 = EDGE_CURVE ( 'NONE', #22614, #11141, #11900, .T. ) ;
#9379 = CARTESIAN_POINT ( 'NONE',  ( 141.0602533517877362, -3576.996034928207791, 2249.541273427662873 ) ) ;
#9380 = ORIENTED_EDGE ( 'NONE', *, *, #22596, .F. ) ;
#9381 = APPLIED_APPROVAL_ASSIGNMENT ( #17811, ( #7499 ) ) ;
#9382 = CARTESIAN_POINT ( 'NONE',  ( 134.4872152579750377, -3577.152335362136455, 2245.116748440663287 ) ) ;
#9383 = CIRCLE ( 'NONE', #765, 2.844800000000091700 ) ;
#9384 = ORIENTED_EDGE ( 'NONE', *, *, #14297, .T. ) ;
#9385 = DIRECTION ( 'NONE',  ( -1.000000000000000000, 0.000000000000000000, 0.000000000000000000 ) ) ;
#9386 = ORIENTED_EDGE ( 'NONE', *, *, #11677, .F. ) ;
#9387 = DIRECTION ( 'NONE',  ( 1.224646799147353207E-16, 1.000000000000000000, -0.000000000000000000 ) ) ;
#9388 = CARTESIAN_POINT ( 'NONE',  ( 15.51375058686055652, -3543.438632179887918, 2255.088298573608881 ) ) ;
#9389 = VERTEX_POINT ( 'NONE', #10629 ) ;
#9390 = DIRECTION ( 'NONE',  ( 0.000000000000000000, -1.000000000000000000, 0.000000000000000000 ) ) ;
#9391 = CARTESIAN_POINT ( 'NONE',  ( 10.46794630892000022, -3597.723865433999890, 2279.591814147000150 ) ) ;
#9392 = EDGE_CURVE ( 'NONE', #12110, #2146, #8157, .T. ) ;
#9393 = ORIENTED_EDGE ( 'NONE', *, *, #2691, .F. ) ;
#9394 = EDGE_CURVE ( 'NONE', #10901, #14851, #21257, .T. ) ;
#9395 = FACE_OUTER_BOUND ( 'NONE', #16100, .T. ) ;
#9396 = CARTESIAN_POINT ( 'NONE',  ( 15.14732702124904407, -3578.044519771737669, 2250.117477721357773 ) ) ;
#9397 = CARTESIAN_POINT ( 'NONE',  ( 0.000000000000000000, 0.000000000000000000, 0.000000000000000000 ) ) ;
#9398 = SECURITY_CLASSIFICATION ( '', '', #10594 ) ;
#9399 = CARTESIAN_POINT ( 'NONE',  ( 57.14999999999999858, -3544.570000000000164, 2244.547199999999975 ) ) ;
#9400 = ORIENTED_EDGE ( 'NONE', *, *, #12293, .T. ) ;
#9401 = APPROVAL_PERSON_ORGANIZATION ( #4861, #4630, #17385 ) ;
#9402 = CARTESIAN_POINT ( 'NONE',  ( 9.987313202740898177, -3661.071170452786646, 2239.009999999999764 ) ) ;
#9403 = APPROVAL_ROLE ( '' ) ;
#9404 = CARTESIAN_POINT ( 'NONE',  ( 142.0316867971999955, -3580.841199999999844, 2242.820000000000164 ) ) ;
#9405 = CARTESIAN_POINT ( 'NONE',  ( -6.730999999999872863, -3654.679000000000087, 2247.392000000000280 ) ) ;
#9406 = ORIENTED_EDGE ( 'NONE', *, *, #18272, .F. ) ;
#9407 = CARTESIAN_POINT ( 'NONE',  ( 18.16297020592579514, -3581.174070066103923, 2245.736054050092662 ) ) ;
#9408 = CARTESIAN_POINT ( 'NONE',  ( 136.8552000000009912, -3579.306319665158753, 2257.962944264954785 ) ) ;
#9409 = AXIS2_PLACEMENT_3D ( 'NONE', #12469, #12238, #17734 ) ;
#9410 = ORIENTED_EDGE ( 'NONE', *, *, #9273, .F. ) ;
#9411 = ORIENTED_EDGE ( 'NONE', *, *, #7661, .T. ) ;
#9412 = CARTESIAN_POINT ( 'NONE',  ( 139.8351778257380431, -3662.349770900797466, 2249.183591361917934 ) ) ;
#9413 = ORIENTED_EDGE ( 'NONE', *, *, #18162, .F. ) ;
#9414 = APPLIED_SECURITY_CLASSIFICATION_ASSIGNMENT ( #9761, ( #23179 ) ) ;
#9415 = VERTEX_POINT ( 'NONE', #6491 ) ;
#9416 = DIRECTION ( 'NONE',  ( 0.000000000000000000, 1.000000000000000000, 0.000000000000000000 ) ) ;
#9417 = VERTEX_POINT ( 'NONE', #9871 ) ;
#9418 = CARTESIAN_POINT ( 'NONE',  ( -5.588000000000000078, -3694.938000000000102, 2229.612000000000080 ) ) ;
#9419 = CALENDAR_DATE ( 2026, 26, 10 ) ;
#9420 = DIRECTION ( 'NONE',  ( 0.000000000000000000, 1.000000000000000000, 0.000000000000000000 ) ) ;
#9421 = AXIS2_PLACEMENT_3D ( 'NONE', #11210, #4513, #2638 ) ;
#9422 = ORIENTED_EDGE ( 'NONE', *, *, #8999, .T. ) ;
#9423 = AXIS2_PLACEMENT_3D ( 'NONE', #6022, #18655, #840 ) ;
#9424 = SPHERICAL_SURFACE ( 'NONE', #2491, 0.7620000000000000107 ) ;
#9425 = CARTESIAN_POINT ( 'NONE',  ( 12.69999999999999929, -3596.322499999999764, 2264.841800000000148 ) ) ;
#9426 = COORDINATED_UNIVERSAL_TIME_OFFSET ( 0, 0, .AHEAD. ) ;
#9427 = ADVANCED_FACE ( 'NONE', ( #12854 ), #1800, .T. ) ;
#9428 = EDGE_CURVE ( 'NONE', #2888, #22298, #15158, .T. ) ;
#9429 = DIRECTION ( 'NONE',  ( -1.000000000000000000, 0.000000000000000000, 0.000000000000000000 ) ) ;
#9430 = EDGE_CURVE ( 'NONE', #2000, #8402, #20534, .T. ) ;
#9431 = VERTEX_POINT ( 'NONE', #17020 ) ;
#9432 = CARTESIAN_POINT ( 'NONE',  ( 142.5401018058971090, -3659.315465601250708, 2250.116512621371385 ) ) ;
#9433 = EDGE_CURVE ( 'NONE', #11168, #7880, #17495, .T. ) ;
#9434 = ORIENTED_EDGE ( 'NONE', *, *, #5135, .F. ) ;
#9435 = AXIS2_PLACEMENT_3D ( 'NONE', #19020, #17252, #17136 ) ;
#9436 = CIRCLE ( 'NONE', #16538, 3.606799999999993567 ) ;
#9437 = DIRECTION ( 'NONE',  ( 7.082568872520999671E-14, 3.885294924354999670E-13, 1.000000000000000000 ) ) ;
#9438 = EDGE_CURVE ( 'NONE', #8583, #13205, #20129, .T. ) ;
#9439 = PLANE ( 'NONE',  #7645 ) ;
#9440 = ORIENTED_EDGE ( 'NONE', *, *, #18659, .T. ) ;
#9441 = EDGE_CURVE ( 'NONE', #10242, #3614, #10391, .T. ) ;
#9442 = DIRECTION ( 'NONE',  ( -0.8660254037825932949, -0.5000000000031962211, 5.608020032303961777E-12 ) ) ;
#9443 = EDGE_LOOP ( 'NONE', ( #19034, #22186 ) ) ;
#9444 = CARTESIAN_POINT ( 'NONE',  ( 147.3829786123148438, -3695.048176948414493, 2260.442427088400564 ) ) ;
#9445 = DIRECTION ( 'NONE',  ( 0.5000000000031885605, -0.8660254037825977358, 0.000000000000000000 ) ) ;
#9446 = LINE ( 'NONE', #11200, #18166 ) ;
#9447 = CARTESIAN_POINT ( 'NONE',  ( 139.6999999999999886, -3576.320000000000164, 2245.359999999999673 ) ) ;
#9448 = CARTESIAN_POINT ( 'NONE',  ( 142.2706313854639291, -3544.133557167201616, 2255.697303096545056 ) ) ;
#9449 = LINE ( 'NONE', #5714, #2361 ) ;
#9450 = CIRCLE ( 'NONE', #12441, 0.7620000000000126672 ) ;
#9451 = AXIS2_PLACEMENT_3D ( 'NONE', #11039, #14679, #21822 ) ;
#9452 = LINE ( 'NONE', #7463, #12858 ) ;
#9453 = ORIENTED_EDGE ( 'NONE', *, *, #15232, .F. ) ;
#9454 = DATE_AND_TIME ( #22088, #17596 ) ;
#9455 = CIRCLE ( 'NONE', #8699, 2.844799999998995244 ) ;
#9456 = EDGE_CURVE ( 'NONE', #6511, #8337, #18666, .T. ) ;
#9457 = CARTESIAN_POINT ( 'NONE',  ( 145.1107615082556777, -3657.665077820303395, 2245.989155495581599 ) ) ;
#9458 = CARTESIAN_POINT ( 'NONE',  ( 9.995409801658235338, -3580.378055366828448, 2249.798395734993846 ) ) ;
#9459 = DIRECTION ( 'NONE',  ( -1.224646799147353207E-16, 1.000000000000000000, 0.000000000000000000 ) ) ;
#9460 = EDGE_LOOP ( 'NONE', ( #4073, #7287, #13384, #14860, #2828 ) ) ;
#9461 = CIRCLE ( 'NONE', #4971, 2.873832635400752622 ) ;
#9462 = DIRECTION ( 'NONE',  ( -1.000000000000000000, 0.000000000000000000, 0.000000000000000000 ) ) ;
#9463 = PLANE ( 'NONE',  #17729 ) ;
#9464 = ORIENTED_EDGE ( 'NONE', *, *, #10960, .F. ) ;
#9465 = VECTOR ( 'NONE', #22198, 1000.000000000000000 ) ;
#9466 = DIRECTION ( 'NONE',  ( -0.9999999999992201793, 1.248865928399024183E-06, 0.000000000000000000 ) ) ;
#9467 = CIRCLE ( 'NONE', #836, 1.269999999999882334 ) ;
#9468 = CYLINDRICAL_SURFACE ( 'NONE', #17800, 2.844799999999994444 ) ;
#9469 = ORIENTED_EDGE ( 'NONE', *, *, #3938, .T. ) ;
#9470 = CARTESIAN_POINT ( 'NONE',  ( 19.05000000000000071, -3578.860000000000127, 2247.392000000000280 ) ) ;
#9471 = ORIENTED_EDGE ( 'NONE', *, *, #4207, .F. ) ;
#9472 = FACE_OUTER_BOUND ( 'NONE', #11924, .T. ) ;
#9473 = CARTESIAN_POINT ( 'NONE',  ( 110.6932000000009992, -3594.099999999999909, 2239.009999999999764 ) ) ;
#9474 = VECTOR ( 'NONE', #21227, 1000.000000000000000 ) ;
#9475 = VERTEX_POINT ( 'NONE', #3948 ) ;
#9476 = LINE ( 'NONE', #15100, #22161 ) ;
#9477 = PRODUCT_DEFINITION_CONTEXT ( 'detailed design', #9320, 'design' ) ;
#9478 = VERTEX_POINT ( 'NONE', #7579 ) ;
#9480 = DIRECTION ( 'NONE',  ( 1.000000000000000000, 0.000000000000000000, 0.000000000000000000 ) ) ;
#9479 = CIRCLE ( 'NONE', #5375, 3.175000000000149925 ) ;
#9481 = COORDINATED_UNIVERSAL_TIME_OFFSET ( 0, 0, .AHEAD. ) ;
#9482 = PRODUCT_RELATED_PRODUCT_CATEGORY ( 'detail', '', ( #785 ) ) ;
#9483 = CARTESIAN_POINT ( 'NONE',  ( 13.01510455369313490, -3642.335645362285504, 2279.814648973302610 ) ) ;
#9484 = CARTESIAN_POINT ( 'NONE',  ( 142.2400000000000091, -3580.776127254000130, 2255.774000000000342 ) ) ;
#9485 = CARTESIAN_POINT ( 'NONE',  ( 142.4126867972000241, -3659.504999999999654, 2239.391000000000076 ) ) ;
#9486 = DIRECTION ( 'NONE',  ( 0.000000000000000000, 1.000000000000000000, 0.000000000000000000 ) ) ;
#9487 = EDGE_CURVE ( 'NONE', #6224, #18611, #13385, .T. ) ;
#9488 = CARTESIAN_POINT ( 'NONE',  ( 139.1589808602738856, -3576.701270618950730, 2249.244916196757458 ) ) ;
#9489 = ORIENTED_EDGE ( 'NONE', *, *, #16997, .T. ) ;
#9490 = AXIS2_PLACEMENT_3D ( 'NONE', #5256, #14597, #3923 ) ;
#9491 = EDGE_CURVE ( 'NONE', #8560, #1593, #662, .T. ) ;
#9492 = CARTESIAN_POINT ( 'NONE',  ( 9.987313202835000681, -3597.931329547144287, 2296.591799999999694 ) ) ;
#9493 = ORIENTED_EDGE ( 'NONE', *, *, #13083, .F. ) ;
#9494 = LINE ( 'NONE', #5645, #15507 ) ;
#9495 = CARTESIAN_POINT ( 'NONE',  ( 142.4431999999993366, -3658.626742952568293, 2255.967040000000907 ) ) ;
#9496 = ORIENTED_EDGE ( 'NONE', *, *, #4435, .F. ) ;
#9497 = DIRECTION ( 'NONE',  ( 5.432398939370942693E-28, 1.000000000000000000, 2.336881798971000105E-14 ) ) ;
#9498 = DIRECTION ( 'NONE',  ( -1.122008997397786234E-13, 0.000000000000000000, -1.000000000000000000 ) ) ;
#9499 = SHAPE_REPRESENTATION ( 'Support Ledge', ( #5611 ), #4481 ) ;
#9500 = ORIENTED_EDGE ( 'NONE', *, *, #17556, .F. ) ;
#9501 = DIRECTION ( 'NONE',  ( 0.000000000000000000, 1.000000000000000000, 0.000000000000000000 ) ) ;
#9502 = CARTESIAN_POINT ( 'NONE',  ( 11.95351013509671745, -3576.749823794578788, 2249.299903167124739 ) ) ;
#9503 = CARTESIAN_POINT ( 'NONE',  ( 64.76999999999999602, -3694.938000000000102, 2289.213099999999940 ) ) ;
#9504 = ORIENTED_EDGE ( 'NONE', *, *, #6935, .F. ) ;
#9505 = FACE_OUTER_BOUND ( 'NONE', #17120, .T. ) ;
#9506 = AXIS2_PLACEMENT_3D ( 'NONE', #11577, #13582, #4441 ) ;
#9507 = DATE_AND_TIME ( #16537, #16460 ) ;
#9508 = APPLIED_PERSON_AND_ORGANIZATION_ASSIGNMENT ( #13078, #6291, ( #10108 ) ) ;
#9509 = CARTESIAN_POINT ( 'NONE',  ( 127.0000000000000000, -3660.140000000000327, 2247.392000000000280 ) ) ;
#9510 = FACE_OUTER_BOUND ( 'NONE', #7541, .T. ) ;
#9511 = CARTESIAN_POINT ( 'NONE',  ( 20.56213590047408246, -3543.486725648842821, 2259.993682086426361 ) ) ;
#9512 = CARTESIAN_POINT ( 'NONE',  ( 136.9475604929545227, -3578.751901585129417, 2257.938841419043456 ) ) ;
#9513 = EDGE_CURVE ( 'NONE', #15997, #20116, #7788, .T. ) ;
#9514 = EDGE_LOOP ( 'NONE', ( #9949, #7905, #616, #5392 ) ) ;
#9515 = CARTESIAN_POINT ( 'NONE',  ( 138.0302948368629643, -3661.810155319285059, 2249.696016199272435 ) ) ;
#9516 = EDGE_CURVE ( 'NONE', #22942, #10444, #675, .T. ) ;
#9517 = ORIENTED_EDGE ( 'NONE', *, *, #7949, .F. ) ;
#9518 = VERTEX_POINT ( 'NONE', #14738 ) ;
#9519 = TOROIDAL_SURFACE ( 'NONE', #4288, 1.905000000000000027, 1.270000000000000018 ) ;
#9520 = AXIS2_PLACEMENT_3D ( 'NONE', #21967, #16913, #2518 ) ;
#9521 = DIRECTION ( 'NONE',  ( 0.000000000000000000, -1.000000000000000000, 0.000000000000000000 ) ) ;
#9522 = CIRCLE ( 'NONE', #7647, 0.3809999999999647002 ) ;
#9523 = ORIENTED_EDGE ( 'NONE', *, *, #8688, .F. ) ;
#9524 = DIRECTION ( 'NONE',  ( 0.000000000000000000, 0.000000000000000000, 1.000000000000000000 ) ) ;
#9525 = FACE_OUTER_BOUND ( 'NONE', #2878, .T. ) ;
#9526 = EDGE_CURVE ( 'NONE', #5890, #2318, #10765, .T. ) ;
#9527 = ORIENTED_EDGE ( 'NONE', *, *, #10113, .F. ) ;
#9528 = CARTESIAN_POINT ( 'NONE',  ( 7.192890077382537939, -3657.977450208451501, 2245.543294774859532 ) ) ;
#9529 = DIRECTION ( 'NONE',  ( 1.000000000000000000, 0.000000000000000000, 0.000000000000000000 ) ) ;
#9530 = DIRECTION ( 'NONE',  ( 0.000000000000000000, 1.000000000000000000, 0.000000000000000000 ) ) ;
#9531 = ADVANCED_FACE ( 'NONE', ( #16903 ), #11745, .T. ) ;
#9532 = CARTESIAN_POINT ( 'NONE',  ( 116.8400000000000034, -3568.700000000000273, 2250.236800000000130 ) ) ;
#9533 = DATE_AND_TIME ( #18438, #18369 ) ;
#9534 = CARTESIAN_POINT ( 'NONE',  ( 9.209369265467998389, -3543.299999999999727, 2282.113800000000083 ) ) ;
#9535 = VECTOR ( 'NONE', #6626, 1000.000000000000000 ) ;
#9536 = AXIS2_PLACEMENT_3D ( 'NONE', #5763, #3992, #7503 ) ;
#9537 = DIRECTION ( 'NONE',  ( -2.324635735433000053E-14, 0.000000000000000000, -1.000000000000000000 ) ) ;
#9538 = CARTESIAN_POINT ( 'NONE',  ( 14.61266695128000137, -3657.399152860999493, 2246.630000000000109 ) ) ;
#9539 = AXIS2_PLACEMENT_3D ( 'NONE', #13770, #20913, #4849 ) ;
#9540 = VERTEX_POINT ( 'NONE', #2962 ) ;
#9541 = CARTESIAN_POINT ( 'NONE',  ( -0.7620000000000000107, -3544.061999999999898, 2228.849999999999909 ) ) ;
#9542 = ADVANCED_FACE ( 'NONE', ( #21763 ), #10106, .F. ) ;
#9543 = DIRECTION ( 'NONE',  ( 0.8660254037817868289, -0.5000000000045929927, -1.484475890920977686E-12 ) ) ;
#9544 = ORIENTED_EDGE ( 'NONE', *, *, #12801, .T. ) ;
#9545 = DIRECTION ( 'NONE',  ( 1.000000000000000000, 0.000000000000000000, 0.000000000000000000 ) ) ;
#9546 = ORIENTED_EDGE ( 'NONE', *, *, #18115, .F. ) ;
#9547 = EDGE_CURVE ( 'NONE', #16505, #20980, #3666, .T. ) ;
#9548 = EDGE_CURVE ( 'NONE', #7211, #3298, #16764, .T. ) ;
#9549 = FACE_OUTER_BOUND ( 'NONE', #21599, .T. ) ;
#9550 = ORIENTED_EDGE ( 'NONE', *, *, #10879, .T. ) ;
#9551 = CARTESIAN_POINT ( 'NONE',  ( 12.69999999999999929, -3597.592500000000200, 2264.841800000000148 ) ) ;
#9552 = AXIS2_PLACEMENT_3D ( 'NONE', #2214, #2441, #17703 ) ;
#9553 = DIRECTION ( 'NONE',  ( -0.8660254037817188832, 0.5000000000047110094, 3.181634500920069822E-14 ) ) ;
#9554 = TOROIDAL_SURFACE ( 'NONE', #3954, 3.606799999999999784, 0.7620000000000000107 ) ;
#9555 = FACE_OUTER_BOUND ( 'NONE', #18340, .T. ) ;
#9556 = AXIS2_PLACEMENT_3D ( 'NONE', #18947, #15319, #15434 ) ;
#9557 = DIRECTION ( 'NONE',  ( -1.000000000000000000, 0.000000000000000000, 0.000000000000000000 ) ) ;
#9558 = AXIS2_PLACEMENT_3D ( 'NONE', #16305, #21808, #18174 ) ;
#9559 = DIRECTION ( 'NONE',  ( 0.000000000000000000, -1.000000000000000000, 0.000000000000000000 ) ) ;
#9560 = CARTESIAN_POINT ( 'NONE',  ( 10.36831320286038149, -3658.158799999850999, 2239.167815367355615 ) ) ;
#9561 = DIRECTION ( 'NONE',  ( -1.000000000000000000, 0.000000000000000000, 0.000000000000000000 ) ) ;
#9562 = VERTEX_POINT ( 'NONE', #15969 ) ;
#9563 = CALENDAR_DATE ( 2026, 26, 10 ) ;
#9564 = CARTESIAN_POINT ( 'NONE',  ( 145.0933512042157645, -3657.614374765385946, 2246.082311836971712 ) ) ;
#9565 = EDGE_CURVE ( 'NONE', #8583, #22551, #12454, .T. ) ;
#9566 = DIRECTION ( 'NONE',  ( 0.000000000000000000, 0.000000000000000000, 1.000000000000000000 ) ) ;
#9567 = CARTESIAN_POINT ( 'NONE',  ( 15.03168679710930178, -3580.841200000109893, 2239.391000000000076 ) ) ;
#9568 = VECTOR ( 'NONE', #314, 1000.000000000000000 ) ;
#9569 = ORIENTED_EDGE ( 'NONE', *, *, #7280, .F. ) ;
#9570 = AXIS2_PLACEMENT_3D ( 'NONE', #14375, #19999, #5823 ) ;
#9571 = CARTESIAN_POINT ( 'NONE',  ( 116.8400000000000034, -3568.700000000000273, 2247.392000000000280 ) ) ;
#9572 = VERTEX_POINT ( 'NONE', #3427 ) ;
#9573 = VECTOR ( 'NONE', #22583, 1000.000000000000000 ) ;
#9574 = CIRCLE ( 'NONE', #19687, 3.606799999999993567 ) ;
#9575 = DIRECTION ( 'NONE',  ( 0.000000000000000000, 0.000000000000000000, 1.000000000000000000 ) ) ;
#9576 = ORIENTED_EDGE ( 'NONE', *, *, #12076, .T. ) ;
#9577 = AXIS2_PLACEMENT_3D ( 'NONE', #1770, #8916, #22963 ) ;
#9578 = CARTESIAN_POINT ( 'NONE',  ( 13.53726674519237250, -3662.223867174984662, 2249.328617614321047 ) ) ;
#9579 = EDGE_CURVE ( 'NONE', #22364, #20612, #5942, .T. ) ;
#9580 = DIRECTION ( 'NONE',  ( 0.000000000000000000, -1.000000000000000000, 0.000000000000000000 ) ) ;
#9581 = AXIS2_PLACEMENT_3D ( 'NONE', #10542, #22600, #20861 ) ;
#9582 = VERTEX_POINT ( 'NONE', #7075 ) ;
#9583 = CARTESIAN_POINT ( 'NONE',  ( 63.50000000000000000, -3594.099999999999909, 2260.600000000000364 ) ) ;
#9584 = B_SPLINE_CURVE_WITH_KNOTS ( 'NONE', 3,
 ( #22404, #9655, #9432, #12943, #20210, #16794, #736, #20101, #16570, #7665, #14825, #5925, #11405, #4151, #2397, #16683, #20649, #6729, #11988, #4727, #15632, #13867, #13758, #10461, #8710, #11875, #8486, #6845, #21018, #22641, #19259, #6380, #11747, #1198, #22868, #9994, #15502, #1082, #1317, #15744, #17362, #12226, #13509, #20902, #3078, #4957, #8242, #6494, #12106, #4835, #8365, #19141, #22760, #6619, #3195, #5082, #10230, #19023, #13629, #10344, #17492, #13987, #1437, #19373, #8595, #21134, #3310 ),
 .UNSPECIFIED., .F., .F.,
 ( 4, 2, 1, 1, 2, 2, 2, 1, 1, 2, 2, 2, 2, 1, 1, 1, 2, 2, 2, 2, 1, 2, 2, 2, 2, 1, 1, 2, 2, 2, 2, 2, 2, 2, 2, 1, 2, 2, 4 ),
 ( 0.000000000000000000, 0.06249999999687816388, 0.09374999999549321616, 0.1093749999946744406, 0.1171874999942121715, 0.1249999999937499023, 0.1874999999894321756, 0.2187499999871572731, 0.2343749999860897937, 0.2421874999855584409, 0.2499999999850270604, 0.3124999999787857474, 0.3437499999755888047, 0.3593749999739168088, 0.3671874999730100342, 0.3710937499726200128, 0.3730468749724225042, 0.3749999999722250510, 0.4062499999690292740, 0.4218749999673663265, 0.4296874999666068784, 0.4335937499661114414, 0.4374999999656160043, 0.4687499999620942659, 0.4843749999603362832, 0.4921874999596303479, 0.4960937499594011424, 0.4980468749594834654, 0.4999999999595658440, 0.5624999999646774773, 0.5937499999673057083, 0.6093749999686635110, 0.6249999999700213138, 0.7499999999813724560, 0.8124999999870490264, 0.8437499999897181135, 0.8593749999908758541, 0.8749999999920334837, 1.000000000000000000 ),
 .UNSPECIFIED. ) ;
#9585 = CARTESIAN_POINT ( 'NONE',  ( -8.890000000022000748, -3580.206200000000081, 2245.060313203000078 ) ) ;
#9586 = ORIENTED_EDGE ( 'NONE', *, *, #17142, .T. ) ;
#9587 = CARTESIAN_POINT ( 'NONE',  ( 95.25000000000000000, -3694.430000000000291, 2243.277199999999993 ) ) ;
#9588 = DIRECTION ( 'NONE',  ( 0.000000000000000000, 1.000000000000000000, 0.000000000000000000 ) ) ;
#9589 = ORIENTED_EDGE ( 'NONE', *, *, #18567, .T. ) ;
#9590 = AXIS2_PLACEMENT_3D ( 'NONE', #11534, #10012, #20341 ) ;
#9591 = CIRCLE ( 'NONE', #17764, 3.606800000000021100 ) ;
#9592 = ORIENTED_EDGE ( 'NONE', *, *, #15296, .T. ) ;
#9593 = AXIS2_PLACEMENT_3D ( 'NONE', #14999, #22132, #6102 ) ;
#9594 = DIRECTION ( 'NONE',  ( 0.000000000000000000, 1.000000000000000000, 0.000000000000000000 ) ) ;
#9595 = ORIENTED_EDGE ( 'NONE', *, *, #1701, .T. ) ;
#9596 = DIRECTION ( 'NONE',  ( 0.000000000000000000, 2.336881798971000105E-14, -1.000000000000000000 ) ) ;
#9597 = AXIS2_PLACEMENT_3D ( 'NONE', #9541, #12719, #2290 ) ;
#9598 = DATE_AND_TIME ( #16620, #6757 ) ;
#9599 = ADVANCED_FACE ( 'NONE', ( #4832 ), #17844, .F. ) ;
#9600 = DIRECTION ( 'NONE',  ( 0.000000000000000000, 0.000000000000000000, -1.000000000000000000 ) ) ;
#9601 = CARTESIAN_POINT ( 'NONE',  ( 17.62147847323069172, -3662.410506574471583, 2245.677565646850780 ) ) ;
#9602 = FACE_OUTER_BOUND ( 'NONE', #16653, .T. ) ;
#9603 = CARTESIAN_POINT ( 'NONE',  ( 9.855200508358999301, -3579.403078924000511, 2257.962940201000038 ) ) ;
#9604 = ORIENTED_EDGE ( 'NONE', *, *, #16409, .F. ) ;
#9605 = CARTESIAN_POINT ( 'NONE',  ( -12.31900000000011985, -3578.860000000000127, 2242.311999999999898 ) ) ;
#9606 = VECTOR ( 'NONE', #31, 1000.000000000000000 ) ;
#9607 = ORIENTED_EDGE ( 'NONE', *, *, #8437, .F. ) ;
#9608 = CARTESIAN_POINT ( 'NONE',  ( 136.9568000000001291, -3578.616742952567620, 2255.967039999999997 ) ) ;
#9609 = EDGE_LOOP ( 'NONE', ( #12326, #16192, #10967, #7504 ) ) ;
#9610 = DIRECTION ( 'NONE',  ( 1.000000000000000000, 0.000000000000000000, 0.000000000000000000 ) ) ;
#9611 = AXIS2_PLACEMENT_3D ( 'NONE', #10288, #2911, #5024 ) ;
#9612 = CARTESIAN_POINT ( 'NONE',  ( 15.24000000016591727, -3544.253380977658708, 2255.773999999824809 ) ) ;
#9613 = APPLIED_PERSON_AND_ORGANIZATION_ASSIGNMENT ( #16215, #8839, ( #9398 ) ) ;
#9614 = ORIENTED_EDGE ( 'NONE', *, *, #8810, .T. ) ;
#9615 = ORIENTED_EDGE ( 'NONE', *, *, #3784, .T. ) ;
#9616 = CARTESIAN_POINT ( 'NONE',  ( 50.79999999999999716, -3670.300000000000182, 2259.837999999999738 ) ) ;
#9617 = ORIENTED_EDGE ( 'NONE', *, *, #10353, .F. ) ;
#9618 = APPLICATION_CONTEXT ( 'configuration controlled 3d designs of mechanical parts and assemblies' ) ;
#9619 = CARTESIAN_POINT ( 'NONE',  ( -12.70000000000005080, -3663.272340905245528, 2247.392000000001644 ) ) ;
#9620 = CARTESIAN_POINT ( 'NONE',  ( 14.29432915190223419, -3577.137138884523665, 2249.656628075460503 ) ) ;
#9621 = CARTESIAN_POINT ( 'NONE',  ( 141.4881110317870423, -3581.707777077976971, 2247.291309677514619 ) ) ;
#9622 = ORIENTED_EDGE ( 'NONE', *, *, #3055, .F. ) ;
#9623 = CARTESIAN_POINT ( 'NONE',  ( 137.0014613743315408, -3660.424486175735638, 2257.925021614027628 ) ) ;
#9624 = COORDINATED_UNIVERSAL_TIME_OFFSET ( 0, 0, .AHEAD. ) ;
#9625 = AXIS2_PLACEMENT_3D ( 'NONE', #18183, #5306, #14674 ) ;
#9626 = DIRECTION ( 'NONE',  ( 0.000000000000000000, 1.000000000000000000, 0.000000000000000000 ) ) ;
#9627 = ORIENTED_EDGE ( 'NONE', *, *, #1169, .T. ) ;
#9628 = FACE_OUTER_BOUND ( 'NONE', #3440, .T. ) ;
#9629 = AXIS2_PLACEMENT_3D ( 'NONE', #9901, #878, #4871 ) ;
#9630 = CARTESIAN_POINT ( 'NONE',  ( 12.69999999999999929, -3585.971999999999753, 2275.055139999999483 ) ) ;
#9631 = CIRCLE ( 'NONE', #7765, 3.606799999999993567 ) ;
#9632 = ORIENTED_EDGE ( 'NONE', *, *, #14397, .T. ) ;
#9633 = CARTESIAN_POINT ( 'NONE',  ( 15.03168679717000167, -3660.851200000000063, 2242.820000000000164 ) ) ;
#9634 = VERTEX_POINT ( 'NONE', #21253 ) ;
#9635 = ORIENTED_EDGE ( 'NONE', *, *, #2510, .T. ) ;
#9636 = PRODUCT_DEFINITION ( 'UNKNOWN', '', #7485, #6692 ) ;
#9637 = AXIS2_PLACEMENT_3D ( 'NONE', #1604, #5140, #3479 ) ;
#9638 = DIRECTION ( 'NONE',  ( -1.224646799147353207E-16, 1.000000000000000000, 0.000000000000000000 ) ) ;
#9639 = ORIENTED_EDGE ( 'NONE', *, *, #10371, .T. ) ;
#9640 = ORIENTED_EDGE ( 'NONE', *, *, #15830, .F. ) ;
#9641 = DIRECTION ( 'NONE',  ( -2.639068250487999990E-12, 1.000000000000000000, 0.000000000000000000 ) ) ;
#9642 = DIRECTION ( 'NONE',  ( 0.000000000000000000, 0.000000000000000000, -1.000000000000000000 ) ) ;
#9643 = ORIENTED_EDGE ( 'NONE', *, *, #20844, .T. ) ;
#9644 = CIRCLE ( 'NONE', #6667, 2.844800000000091700 ) ;
#9645 = CARTESIAN_POINT ( 'NONE',  ( 7.025241774765377478, -3658.828171944931455, 2244.867706167576216 ) ) ;
#9646 = ADVANCED_FACE ( 'NONE', ( #17361 ), #11986, .T. ) ;
#9647 = DIRECTION ( 'NONE',  ( 0.000000000000000000, 0.000000000000000000, -1.000000000000000000 ) ) ;
#9648 = DIRECTION ( 'NONE',  ( -1.000000000000000000, 0.000000000000000000, 0.000000000000000000 ) ) ;
#9649 = ADVANCED_FACE ( 'NONE', ( #6727 ), #6957, .T. ) ;
#9650 = DIRECTION ( 'NONE',  ( 0.000000000000000000, 1.000000000000000000, 0.000000000000000000 ) ) ;
#9651 = SECURITY_CLASSIFICATION_LEVEL ( 'unclassified' ) ;
#9652 = EDGE_CURVE ( 'NONE', #20457, #11664, #6307, .T. ) ;
#9653 = DIRECTION ( 'NONE',  ( -1.000000000000000000, 0.000000000000000000, 0.000000000000000000 ) ) ;
#9654 = ORIENTED_EDGE ( 'NONE', *, *, #12250, .T. ) ;
#9655 = CARTESIAN_POINT ( 'NONE',  ( 142.5447969220999767, -3659.410301963842812, 2250.143339135433507 ) ) ;
#9656 = VECTOR ( 'NONE', #13038, 1000.000000000000000 ) ;
#9657 = CARTESIAN_POINT ( 'NONE',  ( 72.59320000000001016, -3568.700000000000273, 2239.771999999999935 ) ) ;
#9658 = ADVANCED_FACE ( 'NONE', ( #5197 ), #12336, .F. ) ;
#9659 = ORIENTED_EDGE ( 'NONE', *, *, #11389, .F. ) ;
#9660 = LINE ( 'NONE', #16458, #11848 ) ;
#9661 = ADVANCED_FACE ( 'NONE', ( #5076 ), #15630, .T. ) ;
#9662 = CARTESIAN_POINT ( 'NONE',  ( 139.6999999999999886, -3664.965999999999894, 2245.359999999999673 ) ) ;
#9663 = VERTEX_POINT ( 'NONE', #3538 ) ;
#9664 = FACE_OUTER_BOUND ( 'NONE', #20791, .T. ) ;
#9665 = DIRECTION ( 'NONE',  ( -1.000000000000000000, 0.000000000000000000, 0.000000000000000000 ) ) ;
#9666 = ORIENTED_EDGE ( 'NONE', *, *, #17249, .T. ) ;
#9667 = ORIENTED_EDGE ( 'NONE', *, *, #12583, .F. ) ;
#9668 = CARTESIAN_POINT ( 'NONE',  ( 10.36831320290272984, -3638.156299999887324, 2296.210799999999836 ) ) ;
#9669 = DIRECTION ( 'NONE',  ( 0.8660254037841628172, 0.5000000000004778400, -5.443078266502769467E-12 ) ) ;
#9670 = CARTESIAN_POINT ( 'NONE',  ( 15.41268679713999923, -3641.068670452999868, 2296.591799999999694 ) ) ;
#9671 = DIRECTION ( 'NONE',  ( 1.000000000000000000, 0.000000000000000000, 0.000000000000000000 ) ) ;
#9672 = CYLINDRICAL_SURFACE ( 'NONE', #8343, 2.844800000000091700 ) ;
#9673 = DIRECTION ( 'NONE',  ( -1.000000000000000000, 0.000000000000000000, 2.324635735433000053E-14 ) ) ;
#9674 = AXIS2_PLACEMENT_3D ( 'NONE', #4882, #6772, #18950 ) ;
#9675 = CARTESIAN_POINT ( 'NONE',  ( 20.42971111056401767, -3695.268694217237226, 2260.325313175604151 ) ) ;
#9676 = EDGE_CURVE ( 'NONE', #11901, #11706, #2930, .T. ) ;
#9677 = ORIENTED_EDGE ( 'NONE', *, *, #22299, .F. ) ;
#9678 = DATE_AND_TIME ( #9563, #22093 ) ;
#9679 = EDGE_CURVE ( 'NONE', #3220, #14115, #4419, .T. ) ;
#9680 = ORIENTED_EDGE ( 'NONE', *, *, #6803, .T. ) ;
#9681 = DIRECTION ( 'NONE',  ( 1.273565328809000167E-14, 1.000000000000000000, -1.319970543219000025E-14 ) ) ;
#9682 = DIRECTION ( 'NONE',  ( 0.000000000000000000, 0.000000000000000000, -1.000000000000000000 ) ) ;
#9683 = DIRECTION ( 'NONE',  ( 1.000000000000000000, 0.000000000000000000, 0.000000000000000000 ) ) ;
#9684 = VERTEX_POINT ( 'NONE', #3191 ) ;
#9685 = DIRECTION ( 'NONE',  ( 0.000000000000000000, 0.000000000000000000, -1.000000000000000000 ) ) ;
#9686 = FACE_OUTER_BOUND ( 'NONE', #12154, .T. ) ;
#9687 = ORIENTED_EDGE ( 'NONE', *, *, #16004, .F. ) ;
#9688 = CIRCLE ( 'NONE', #9319, 2.844800000000001550 ) ;
#9689 = CARTESIAN_POINT ( 'NONE',  ( -8.890000000022000748, -3580.206200000000081, 2245.060313203000078 ) ) ;
#9690 = CARTESIAN_POINT ( 'NONE',  ( 14.46545461912941022, -3661.735746247042243, 2249.747105226763779 ) ) ;
#9691 = LINE ( 'NONE', #15203, #13316 ) ;
#9692 = ORIENTED_EDGE ( 'NONE', *, *, #6832, .T. ) ;
#9693 = FACE_OUTER_BOUND ( 'NONE', #16791, .T. ) ;
#9694 = CARTESIAN_POINT ( 'NONE',  ( 15.11851230223999920, -3637.993080951000593, 2279.551734718999796 ) ) ;
#9695 = CARTESIAN_POINT ( 'NONE',  ( 114.2999999999999972, -3644.899999999999636, 2261.869999999999891 ) ) ;
#9696 = CARTESIAN_POINT ( 'NONE',  ( 25.39999999999999858, -3670.300000000000182, 2259.837999999999738 ) ) ;
#9697 = ORIENTED_EDGE ( 'NONE', *, *, #11116, .F. ) ;
#9698 = ORIENTED_EDGE ( 'NONE', *, *, #22934, .T. ) ;
#9699 = AXIS2_PLACEMENT_3D ( 'NONE', #6874, #8622, #3457 ) ;
#9700 = CARTESIAN_POINT ( 'NONE',  ( 137.2104978356084075, -3580.932314744983614, 2239.009999999967931 ) ) ;
#9701 = EDGE_LOOP ( 'NONE', ( #18524, #10350, #22140, #13700 ) ) ;
#9702 = VECTOR ( 'NONE', #16812, 1000.000000000000000 ) ;
#9703 = CARTESIAN_POINT ( 'NONE',  ( 145.2664576437646815, -3580.789478182276071, 2245.301509789881493 ) ) ;
#9704 = APPROVAL_ROLE ( '' ) ;
#9705 = EDGE_CURVE ( 'NONE', #5314, #1446, #1263, .T. ) ;
#9706 = ADVANCED_FACE ( 'NONE', ( #12799 ), #3769, .T. ) ;
#9707 = CARTESIAN_POINT ( 'NONE',  ( 13.32717070831999884, -3642.283331859000100, 2279.801370659999975 ) ) ;
#9708 = EDGE_CURVE ( 'NONE', #19068, #21395, #10925, .T. ) ;
#9709 = CARTESIAN_POINT ( 'NONE',  ( 17.57087389318388659, -3662.494267584890622, 2245.794996442214597 ) ) ;
#9710 = DIRECTION ( 'NONE',  ( 0.000000000000000000, 0.000000000000000000, -1.000000000000000000 ) ) ;
#9711 = CARTESIAN_POINT ( 'NONE',  ( 12.69999999999999929, -3576.650200000000041, 2257.592639999999847 ) ) ;
#9712 = DIRECTION ( 'NONE',  ( 1.000000000000000000, 0.000000000000000000, 0.000000000000000000 ) ) ;
#9713 = EDGE_CURVE ( 'NONE', #14933, #11901, #5133, .T. ) ;
#9714 = EDGE_LOOP ( 'NONE', ( #15112, #14067 ) ) ;
#9715 = FACE_OUTER_BOUND ( 'NONE', #22834, .T. ) ;
#9716 = FACE_OUTER_BOUND ( 'NONE', #7587, .T. ) ;
#9717 = EDGE_LOOP ( 'NONE', ( #5862, #2767, #14349, #23107 ) ) ;
#9718 = APPLIED_APPROVAL_ASSIGNMENT ( #1322, ( #7485 ) ) ;
#9719 = CARTESIAN_POINT ( 'NONE',  ( 18.41519309054999809, -3659.710859637462363, 2244.571829071724096 ) ) ;
#9720 = VECTOR ( 'NONE', #7781, 1000.000000000000000 ) ;
#9721 = CARTESIAN_POINT ( 'NONE',  ( 10.87796901928627058, -3657.320223683514996, 2246.982647036138587 ) ) ;
#9722 = EDGE_CURVE ( 'NONE', #15033, #16863, #23108, .T. ) ;
#9723 = ORIENTED_EDGE ( 'NONE', *, *, #11514, .F. ) ;
#9724 = EDGE_CURVE ( 'NONE', #8952, #4017, #19775, .T. ) ;
#9725 = EDGE_LOOP ( 'NONE', ( #18478, #65, #22329, #11018 ) ) ;
#9726 = CARTESIAN_POINT ( 'NONE',  ( -5.588000000000000078, -3694.938000000000102, 2228.849999999999909 ) ) ;
#9727 = ORIENTED_EDGE ( 'NONE', *, *, #526, .T. ) ;
#9728 = CARTESIAN_POINT ( 'NONE',  ( -12.31899999999987116, -3660.140000000000327, 2252.853000000000065 ) ) ;
#9729 = CARTESIAN_POINT ( 'NONE',  ( 15.28019367547714680, -3578.294426589508930, 2250.180878883692458 ) ) ;
#9730 = CARTESIAN_POINT ( 'NONE',  ( 0.000000000000000000, 0.000000000000000000, 0.000000000000000000 ) ) ;
#9731 = CARTESIAN_POINT ( 'NONE',  ( 142.3050992937297110, -3580.638258740797937, 2249.612730726536029 ) ) ;
#9732 = ORIENTED_EDGE ( 'NONE', *, *, #19582, .F. ) ;
#9733 = DIRECTION ( 'NONE',  ( -1.000000000000000000, 0.000000000000000000, 0.000000000000000000 ) ) ;
#9734 = PERSON_AND_ORGANIZATION_ROLE ( 'classification_officer' ) ;
#9735 = CARTESIAN_POINT ( 'NONE',  ( 1.270000000000000018, -3694.430000000000291, 2259.329999999999927 ) ) ;
#9736 = APPLIED_APPROVAL_ASSIGNMENT ( #176, ( #2620 ) ) ;
#9737 = CARTESIAN_POINT ( 'NONE',  ( 20.70572851130767233, -3543.336642707656665, 2259.634237443121492 ) ) ;
#9738 = DIRECTION ( 'NONE',  ( 1.000000000000000000, 0.000000000000000000, 0.000000000000000000 ) ) ;
#9739 = EDGE_LOOP ( 'NONE', ( #622, #1465, #15692, #7422 ) ) ;
#9740 = CARTESIAN_POINT ( 'NONE',  ( -12.31900000000000084, -3580.206200000121044, 2249.723686796789480 ) ) ;
#9741 = ORIENTED_EDGE ( 'NONE', *, *, #3799, .F. ) ;
#9742 = ORIENTED_EDGE ( 'NONE', *, *, #22718, .F. ) ;
#9743 = CARTESIAN_POINT ( 'NONE',  ( -0.7620000000000000107, -3695.699999999999818, 2253.487999999999829 ) ) ;
#9744 = EDGE_LOOP ( 'NONE', ( #5905, #8596, #21355, #3042 ) ) ;
#9745 = LOCAL_TIME ( 17, 37, 43.00000000000000000, #9116 ) ;
#9746 = CYLINDRICAL_SURFACE ( 'NONE', #9769, 6.349999999999855760 ) ;
#9747 = DIRECTION ( 'NONE',  ( 1.000000000000000000, 0.000000000000000000, 0.000000000000000000 ) ) ;
#9748 = LOCAL_TIME ( 17, 37, 43.00000000000000000, #7690 ) ;
#9749 = ORIENTED_EDGE ( 'NONE', *, *, #16965, .T. ) ;
#9750 = DIRECTION ( 'NONE',  ( 0.000000000000000000, 1.000000000000000000, 0.000000000000000000 ) ) ;
#9751 = DIRECTION ( 'NONE',  ( 0.000000000000000000, 0.000000000000000000, 1.000000000000000000 ) ) ;
#9752 = CARTESIAN_POINT ( 'NONE',  ( 61.26424768829000556, -3694.938000000000102, 2279.827800000000025 ) ) ;
#9753 = CARTESIAN_POINT ( 'NONE',  ( 12.69999999999999929, -3659.504999999999654, 2239.009999999999764 ) ) ;
#9754 = PERSON_AND_ORGANIZATION ( #5446, #1895 ) ;
#9755 = AXIS2_PLACEMENT_3D ( 'NONE', #16468, #18341, #14498 ) ;
#9756 = DIRECTION ( 'NONE',  ( 0.000000000000000000, 0.000000000000000000, -1.000000000000000000 ) ) ;
#9757 = DIRECTION ( 'NONE',  ( -1.000000000000000000, 0.000000000000000000, 0.000000000000000000 ) ) ;
#9758 = APPLIED_PERSON_AND_ORGANIZATION_ASSIGNMENT ( #13034, #21702, ( #10100 ) ) ;
#9759 = LINE ( 'NONE', #11186, #21440 ) ;
#9760 = FACE_OUTER_BOUND ( 'NONE', #11025, .T. ) ;
#9761 = SECURITY_CLASSIFICATION ( '', '', #5796 ) ;
#9762 = EDGE_LOOP ( 'NONE', ( #15700, #16777, #11587, #9504 ) ) ;
#9763 = DIRECTION ( 'NONE',  ( -2.286657950257999976E-13, 0.000000000000000000, 1.000000000000000000 ) ) ;
#9764 = EDGE_CURVE ( 'NONE', #2236, #22803, #14568, .T. ) ;
#9765 = ORIENTED_EDGE ( 'NONE', *, *, #22885, .T. ) ;
#9766 = AXIS2_PLACEMENT_3D ( 'NONE', #16817, #4062, #15189 ) ;
#9767 = CARTESIAN_POINT ( 'NONE',  ( 142.3973403485965719, -3580.417758129517097, 2257.924723937801900 ) ) ;
#9768 = EDGE_CURVE ( 'NONE', #7518, #5042, #21932, .T. ) ;
#9769 = AXIS2_PLACEMENT_3D ( 'NONE', #22392, #7887, #13389 ) ;
#9770 = CARTESIAN_POINT ( 'NONE',  ( 105.2067999999999870, -3568.700000000000273, 2239.771999999999935 ) ) ;
#9771 = ORIENTED_EDGE ( 'NONE', *, *, #15101, .T. ) ;
#9772 = ORIENTED_EDGE ( 'NONE', *, *, #9000, .T. ) ;
#9773 = FACE_OUTER_BOUND ( 'NONE', #18425, .T. ) ;
#9774 = DIRECTION ( 'NONE',  ( 0.000000000000000000, 0.000000000000000000, -1.000000000000000000 ) ) ;
#9775 = FACE_OUTER_BOUND ( 'NONE', #21417, .T. ) ;
#9776 = DIRECTION ( 'NONE',  ( 0.000000000000000000, 0.000000000000000000, 1.000000000000000000 ) ) ;
#9777 = DIRECTION ( 'NONE',  ( -1.000000000000000000, 0.000000000000000000, 0.000000000000000000 ) ) ;
#9778 = CARTESIAN_POINT ( 'NONE',  ( 20.75836682411413747, -3695.690215920803439, 2259.501687144741027 ) ) ;
#9779 = ORIENTED_EDGE ( 'NONE', *, *, #5081, .T. ) ;
#9780 = APPROVAL_DATE_TIME ( #6060, #2619 ) ;
#9781 = VERTEX_POINT ( 'NONE', #1793 ) ;
#9782 = LINE ( 'NONE', #7922, #2660 ) ;
#9783 = AXIS2_PLACEMENT_3D ( 'NONE', #7210, #300, #10837 ) ;
#9784 = CIRCLE ( 'NONE', #2326, 3.606800000000000228 ) ;
#9785 = CARTESIAN_POINT ( 'NONE',  ( 22.54063073453000143, -3544.061999999999898, 2275.001800000000003 ) ) ;
#9786 = CYLINDRICAL_SURFACE ( 'NONE', #19815, 3.175000000000149925 ) ;
#9787 = ORIENTED_EDGE ( 'NONE', *, *, #12250, .F. ) ;
#9788 = CARTESIAN_POINT ( 'NONE',  ( 9.855199999999999960, -3579.494999999999891, 2272.030000000000200 ) ) ;
#9789 = EDGE_CURVE ( 'NONE', #14462, #2024, #11041, .T. ) ;
#9790 = ADVANCED_FACE ( 'NONE', ( #8940 ), #16086, .F. ) ;
#9791 = DIRECTION ( 'NONE',  ( 0.000000000000000000, 0.000000000000000000, -1.000000000000000000 ) ) ;
#9792 = DIRECTION ( 'NONE',  ( 2.336881798971000105E-14, 0.000000000000000000, 1.000000000000000000 ) ) ;
#9793 = EDGE_LOOP ( 'NONE', ( #7953, #6397, #1036, #9076 ) ) ;
#9794 = CARTESIAN_POINT ( 'NONE',  ( 40.94480000000000075, -3644.899999999999636, 2239.771999999999935 ) ) ;
#9795 = ADVANCED_FACE ( 'NONE', ( #2147 ), #19726, .F. ) ;
#9796 = CIRCLE ( 'NONE', #19920, 2.844799999999994444 ) ;
#9797 = EDGE_CURVE ( 'NONE', #4689, #3037, #6352, .T. ) ;
#9798 = DIRECTION ( 'NONE',  ( -1.000000000000000000, 0.000000000000000000, 0.000000000000000000 ) ) ;
#9799 = ORIENTED_EDGE ( 'NONE', *, *, #20109, .F. ) ;
#9800 = TOROIDAL_SURFACE ( 'NONE', #16551, 5.080000000000000071, 0.3810000000000000053 ) ;
#9801 = DIRECTION ( 'NONE',  ( 0.000000000000000000, 0.000000000000000000, 1.000000000000000000 ) ) ;
#9802 = TOROIDAL_SURFACE ( 'NONE', #8329, 5.080000000000000071, 0.3810000000000000053 ) ;
#9803 = CARTESIAN_POINT ( 'NONE',  ( 14.47434230490000040, -3637.271017030000166, 2279.676071933000003 ) ) ;
#9804 = CIRCLE ( 'NONE', #823, 0.7619999999999987894 ) ;
#9805 = CARTESIAN_POINT ( 'NONE',  ( 151.4000000000000057, -3660.140000000000327, 2247.392000000000280 ) ) ;
#9806 = DIRECTION ( 'NONE',  ( -1.000000000000000000, 0.000000000000000000, 0.000000000000000000 ) ) ;
#9807 = EDGE_LOOP ( 'NONE', ( #4026, #1909, #3698, #10191, #11367 ) ) ;
#9808 = VERTEX_POINT ( 'NONE', #22379 ) ;
#9809 = AXIS2_PLACEMENT_3D ( 'NONE', #11645, #10019, #13187 ) ;
#9810 = DIRECTION ( 'NONE',  ( 0.000000000000000000, 0.000000000000000000, -1.000000000000000000 ) ) ;
#9811 = ADVANCED_FACE ( 'NONE', ( #8108 ), #315, .T. ) ;
#9812 = ORIENTED_EDGE ( 'NONE', *, *, #6707, .F. ) ;
#9813 = CARTESIAN_POINT ( 'NONE',  ( 136.8552000000009912, -3659.504999999999654, 2272.030000000000200 ) ) ;
#9815 = CIRCLE ( 'NONE', #4221, 0.7619999999999294005 ) ;
#9814 = COORDINATED_UNIVERSAL_TIME_OFFSET ( 0, 0, .AHEAD. ) ;
#9816 = FACE_OUTER_BOUND ( 'NONE', #7911, .T. ) ;
#9817 = CARTESIAN_POINT ( 'NONE',  ( 18.37893127878000143, -3660.140301727999940, 2244.547200027999679 ) ) ;
#9818 = AXIS2_PLACEMENT_3D ( 'NONE', #21274, #12122, #19506 ) ;
#9819 = DIRECTION ( 'NONE',  ( 0.000000000000000000, 0.000000000000000000, -1.000000000000000000 ) ) ;
#9820 = DIRECTION ( 'NONE',  ( -1.000000000000000000, -1.935622821353000237E-14, 0.000000000000000000 ) ) ;
#9821 = VECTOR ( 'NONE', #22750, 1000.000000000000000 ) ;
#9822 = CARTESIAN_POINT ( 'NONE',  ( 63.50000000000000000, -3594.099999999999909, 2239.771999999999935 ) ) ;
#9823 = ORIENTED_EDGE ( 'NONE', *, *, #6105, .F. ) ;
#9824 = CARTESIAN_POINT ( 'NONE',  ( 12.69999999999999929, -3570.287499999999909, 2268.705139999999574 ) ) ;
#9825 = EDGE_CURVE ( 'NONE', #16546, #10242, #1422, .T. ) ;
#9826 = DIRECTION ( 'NONE',  ( 0.000000000000000000, 0.000000000000000000, -1.000000000000000000 ) ) ;
#9827 = VERTEX_POINT ( 'NONE', #11601 ) ;
#9828 = CARTESIAN_POINT ( 'NONE',  ( 15.03168679717000167, -3580.841199999999844, 2239.391000000000076 ) ) ;
#9829 = CARTESIAN_POINT ( 'NONE',  ( 15.40195214416352876, -3543.639179024606165, 2255.368362556376724 ) ) ;
#9830 = AXIS2_PLACEMENT_3D ( 'NONE', #6326, #16969, #4440 ) ;
#9831 = EDGE_CURVE ( 'NONE', #553, #8199, #22493, .T. ) ;
#9832 = ORIENTED_EDGE ( 'NONE', *, *, #2128, .T. ) ;
#9833 = EDGE_CURVE ( 'NONE', #2616, #15095, #11120, .T. ) ;
#9834 = ORIENTED_EDGE ( 'NONE', *, *, #20468, .T. ) ;
#9835 = ORIENTED_EDGE ( 'NONE', *, *, #5148, .F. ) ;
#9836 = DIRECTION ( 'NONE',  ( -1.000000000000000000, 2.330758767201999921E-14, 2.343004830739999973E-14 ) ) ;
#9837 = EDGE_LOOP ( 'NONE', ( #8774, #19104, #190, #11113, #18202, #8464 ) ) ;
#9838 = CLOSED_SHELL ( 'NONE', ( #22646, #1994, #530, #18531, #1228, #384, #21728, #20898, #9790, #4129 ) ) ;
#9839 = CARTESIAN_POINT ( 'NONE',  ( 9.855199999999999960, -3639.502500000000055, 2263.571799999999712 ) ) ;
#9840 = CARTESIAN_POINT ( 'NONE',  ( 14.86805197786120480, -3577.652999197129247, 2249.968111766196216 ) ) ;
#9841 = CARTESIAN_POINT ( 'NONE',  ( 139.6999999999999886, -3668.712499999999636, 2268.705139999999574 ) ) ;
#9842 = EDGE_CURVE ( 'NONE', #18657, #6441, #941, .T. ) ;
#9843 = ORIENTED_EDGE ( 'NONE', *, *, #12964, .F. ) ;
#9844 = DIRECTION ( 'NONE',  ( 0.000000000000000000, -2.336881798971000105E-14, 1.000000000000000000 ) ) ;
#9845 = PERSON_AND_ORGANIZATION_ROLE ( 'creator' ) ;
#9846 = CARTESIAN_POINT ( 'NONE',  ( 38.10000000000000142, -3594.099999999999909, 2260.600000000000364 ) ) ;
#9847 = DIRECTION ( 'NONE',  ( 1.122008997397786234E-13, 0.000000000000000000, -1.000000000000000000 ) ) ;
#9848 = CIRCLE ( 'NONE', #8745, 5.460999999999938126 ) ;
#9849 = EDGE_CURVE ( 'NONE', #21067, #20079, #14112, .T. ) ;
#9850 = DIRECTION ( 'NONE',  ( 0.000000000000000000, 0.000000000000000000, 1.000000000000000000 ) ) ;
#9851 = EDGE_CURVE ( 'NONE', #3037, #18991, #4302, .T. ) ;
#9852 = VECTOR ( 'NONE', #21870, 1000.000000000000000 ) ;
#9853 = ORIENTED_EDGE ( 'NONE', *, *, #4229, .T. ) ;
#9854 = AXIS2_PLACEMENT_3D ( 'NONE', #7410, #14562, #2365 ) ;
#9855 = LINE ( 'NONE', #18879, #10313 ) ;
#9856 = AXIS2_PLACEMENT_3D ( 'NONE', #2683, #22242, #22137 ) ;
#9857 = ORIENTED_EDGE ( 'NONE', *, *, #17445, .F. ) ;
#9858 = ORIENTED_EDGE ( 'NONE', *, *, #6586, .T. ) ;
#9859 = EDGE_CURVE ( 'NONE', #18858, #14398, #16399, .T. ) ;
#9860 = FACE_OUTER_BOUND ( 'NONE', #8181, .T. ) ;
#9861 = EDGE_LOOP ( 'NONE', ( #11508, #6359 ) ) ;
#9862 = DIRECTION ( 'NONE',  ( 1.000000000000000000, 0.000000000000000000, 0.000000000000000000 ) ) ;
#9863 = DIRECTION ( 'NONE',  ( 0.000000000000000000, 1.000000000000000000, 0.000000000000000000 ) ) ;
#9864 = AXIS2_PLACEMENT_3D ( 'NONE', #4330, #18621, #9712 ) ;
#9865 = ORIENTED_EDGE ( 'NONE', *, *, #16471, .T. ) ;
#9866 = CARTESIAN_POINT ( 'NONE',  ( 7.135618720840391838, -3658.201644552495509, 2245.309768844839255 ) ) ;
#9867 = DIRECTION ( 'NONE',  ( -1.000000000000000000, 2.331176954593508450E-12, 0.000000000000000000 ) ) ;
#9868 = CYLINDRICAL_SURFACE ( 'NONE', #12611, 2.844800000000091700 ) ;
#9869 = APPROVAL_ROLE ( '' ) ;
#9870 = DIRECTION ( 'NONE',  ( 0.000000000000000000, -1.000000000000000000, 0.000000000000000000 ) ) ;
#9871 = CARTESIAN_POINT ( 'NONE',  ( 137.3683132029982517, -3658.158799999858729, 2239.391000000000076 ) ) ;
#9872 = EDGE_CURVE ( 'NONE', #18081, #13878, #4008, .T. ) ;
#9873 = CARTESIAN_POINT ( 'NONE',  ( -12.31900000000011985, -3660.140000000000327, 2242.311999999999898 ) ) ;
#9874 = CARTESIAN_POINT ( 'NONE',  ( 0.7620000000000000107, -3544.061999999999898, 2275.001800000000003 ) ) ;
#9875 = ORIENTED_EDGE ( 'NONE', *, *, #13083, .T. ) ;
#9876 = AXIS2_PLACEMENT_3D ( 'NONE', #8192, #15337, #20846 ) ;
#9877 = CARTESIAN_POINT ( 'NONE',  ( 50.79999999999999716, -3670.300000000000182, 2260.600000000000364 ) ) ;
#9878 = VECTOR ( 'NONE', #15901, 1000.000000000000000 ) ;
#9879 = VERTEX_POINT ( 'NONE', #20403 ) ;
#9880 = CARTESIAN_POINT ( 'NONE',  ( 50.79999999999999716, -3568.700000000000273, 2239.771999999999935 ) ) ;
#9881 = FACE_OUTER_BOUND ( 'NONE', #17161, .T. ) ;
#9882 = EDGE_LOOP ( 'NONE', ( #12753, #160, #22116, #19533 ) ) ;
#9883 = EDGE_LOOP ( 'NONE', ( #20099, #3324, #1705, #9208 ) ) ;
#9884 = FACE_OUTER_BOUND ( 'NONE', #18960, .T. ) ;
#9885 = CARTESIAN_POINT ( 'NONE',  ( 20.12315942193000140, -3694.472271328999796, 2260.413001451000127 ) ) ;
#9886 = DIRECTION ( 'NONE',  ( 1.000000000000000000, 0.000000000000000000, 0.000000000000000000 ) ) ;
#9887 = DIRECTION ( 'NONE',  ( 0.000000000000000000, 0.000000000000000000, 1.000000000000000000 ) ) ;
#9888 = DIRECTION ( 'NONE',  ( 1.000000000000000000, 0.000000000000000000, 0.000000000000000000 ) ) ;
#9889 = CARTESIAN_POINT ( 'NONE',  ( 18.37960467573999779, -3578.859731361000286, 2244.547525601999951 ) ) ;
#9890 = AXIS2_PLACEMENT_3D ( 'NONE', #2997, #22904, #6997 ) ;
#9891 = CARTESIAN_POINT ( 'NONE',  ( 64.76999999999999602, -3544.061999999999898, 2289.213099999999940 ) ) ;
#9892 = ORIENTED_EDGE ( 'NONE', *, *, #11984, .F. ) ;
#9893 = PERSON_AND_ORGANIZATION ( #5446, #1895 ) ;
#9894 = ORIENTED_EDGE ( 'NONE', *, *, #2542, .T. ) ;
#9895 = AXIS2_PLACEMENT_3D ( 'NONE', #11890, #3443, #15408 ) ;
#9896 = CARTESIAN_POINT ( 'NONE',  ( 10.16000000000000014, -3578.213872745999652, 2255.774000000000342 ) ) ;
#9897 = DIRECTION ( 'NONE',  ( -1.000000000000000000, 0.000000000000000000, 0.000000000000000000 ) ) ;
#9898 = CARTESIAN_POINT ( 'NONE',  ( 9.855099624826999971, -3659.505002774999411, 2250.165042250000170 ) ) ;
#9899 = ADVANCED_BREP_SHAPE_REPRESENTATION ( '', ( #13990, #5611 ), #5641 ) ;
#9900 = ORIENTED_EDGE ( 'NONE', *, *, #19404, .T. ) ;
#9901 = CARTESIAN_POINT ( 'NONE',  ( 12.69999999999999929, -3583.940000000000055, 2268.705139999999574 ) ) ;
#9902 = CIRCLE ( 'NONE', #4318, 0.7619999999999996776 ) ;
#9903 = CARTESIAN_POINT ( 'NONE',  ( 139.6999999999999886, -3659.504999999999654, 2245.359999999999673 ) ) ;
#9904 = CARTESIAN_POINT ( 'NONE',  ( 144.7839377732694288, -3662.117457879833637, 2245.342794673845219 ) ) ;
#9905 = ORIENTED_EDGE ( 'NONE', *, *, #799, .F. ) ;
#9906 = LINE ( 'NONE', #20472, #6620 ) ;
#9907 = CIRCLE ( 'NONE', #18882, 5.080000000000000959 ) ;
#9908 = CARTESIAN_POINT ( 'NONE',  ( 15.05122374280866815, -3661.108641140468990, 2250.067759433852189 ) ) ;
#9909 = AXIS2_PLACEMENT_3D ( 'NONE', #14752, #21779, #20145 ) ;
#9910 = CARTESIAN_POINT ( 'NONE',  ( 124.1552000000010025, -3568.700000000000273, 2261.869999999999891 ) ) ;
#9911 = AXIS2_PLACEMENT_3D ( 'NONE', #8925, #7065, #3880 ) ;
#9912 = ORIENTED_EDGE ( 'NONE', *, *, #21246, .F. ) ;
#9913 = CARTESIAN_POINT ( 'NONE',  ( 145.0128742528999908, -3581.600847139000052, 2246.630000000000109 ) ) ;
#9914 = CARTESIAN_POINT ( 'NONE',  ( 15.53320999718999929, -3639.188150532000236, 2279.450415100000100 ) ) ;
#9915 = APPLIED_DATE_AND_TIME_ASSIGNMENT ( #15819, #19891, ( #14623 ) ) ;
#9916 = CYLINDRICAL_SURFACE ( 'NONE', #11931, 5.714999999999999858 ) ;
#9917 = CARTESIAN_POINT ( 'NONE',  ( 15.48868721613555977, -3658.939971329327818, 2249.971339383300347 ) ) ;
#9918 = CARTESIAN_POINT ( 'NONE',  ( 15.03168679717000167, -3660.851200000000063, 2239.391000000000076 ) ) ;
#9919 = ORIENTED_EDGE ( 'NONE', *, *, #19878, .F. ) ;
#9920 = ORIENTED_EDGE ( 'NONE', *, *, #7015, .T. ) ;
#9921 = ADVANCED_FACE ( 'NONE', ( #9628 ), #16772, .T. ) ;
#9922 = LINE ( 'NONE', #686, #5767 ) ;
#9923 = ADVANCED_FACE ( 'NONE', ( #16878, #11494 ), #18644, .F. ) ;
#9924 = CIRCLE ( 'NONE', #5845, 1.269999999999882334 ) ;
#9925 = EDGE_LOOP ( 'NONE', ( #11674, #2854, #15695, #4889 ) ) ;
#9926 = CARTESIAN_POINT ( 'NONE',  ( 141.4511983580732704, -3657.232884635242499, 2257.728283137804738 ) ) ;
#9927 = ADVANCED_FACE ( 'NONE', ( #13839 ), #9301, .T. ) ;
#9928 = DIRECTION ( 'NONE',  ( -1.000000000000000000, 0.000000000000000000, 0.000000000000000000 ) ) ;
#9929 = CIRCLE ( 'NONE', #6596, 3.606799999999001027 ) ;
#9930 = DIRECTION ( 'NONE',  ( 1.000000000000000000, 0.000000000000000000, 0.000000000000000000 ) ) ;
#9931 = CARTESIAN_POINT ( 'NONE',  ( 17.69701424773149512, -3662.279354287278238, 2245.514279573343629 ) ) ;
#9932 = AXIS2_PLACEMENT_3D ( 'NONE', #16061, #21110, #5053 ) ;
#9933 = CARTESIAN_POINT ( 'NONE',  ( 15.54479999999999862, -3659.504999999999654, 2256.063560000000052 ) ) ;
#9934 = DIRECTION ( 'NONE',  ( 0.000000000000000000, -1.000000000000000000, 0.000000000000000000 ) ) ;
#9935 = EDGE_CURVE ( 'NONE', #8878, #9083, #22369, .T. ) ;
#9936 = DIRECTION ( 'NONE',  ( 1.000000000000000000, 0.000000000000000000, 3.996303350731721563E-14 ) ) ;
#9937 = VERTEX_POINT ( 'NONE', #17691 ) ;
#9938 = DIRECTION ( 'NONE',  ( 0.000000000000000000, -1.000000000000000000, 0.000000000000000000 ) ) ;
#9939 = CARTESIAN_POINT ( 'NONE',  ( 18.41499999999999915, -3659.504999999999654, 2239.771999999999935 ) ) ;
#9940 = ORIENTED_EDGE ( 'NONE', *, *, #20465, .T. ) ;
#9941 = EDGE_CURVE ( 'NONE', #1484, #10742, #18268, .T. ) ;
#9942 = AXIS2_PLACEMENT_3D ( 'NONE', #12002, #10241, #8729 ) ;
#9943 = CARTESIAN_POINT ( 'NONE',  ( 142.7470794804999912, -3543.299999999999727, 2254.503999999999905 ) ) ;
#9944 = CARTESIAN_POINT ( 'NONE',  ( 10.08643964193837661, -3658.381561134523054, 2249.628385529651496 ) ) ;
#9945 = TOROIDAL_SURFACE ( 'NONE', #15949, 5.080000000000000071, 0.3810000000000000053 ) ;
#9946 = VERTEX_POINT ( 'NONE', #4810 ) ;
#9947 = CIRCLE ( 'NONE', #18192, 2.844799999999999773 ) ;
#9948 = EDGE_LOOP ( 'NONE', ( #2475, #19379, #12958, #16941 ) ) ;
#9949 = ORIENTED_EDGE ( 'NONE', *, *, #21970, .F. ) ;
#9950 = CARTESIAN_POINT ( 'NONE',  ( 12.69999999999999929, -3639.502500000000055, 2295.829799999999977 ) ) ;
#9951 = AXIS2_PLACEMENT_3D ( 'NONE', #6761, #70, #16006 ) ;
#9952 = ORIENTED_EDGE ( 'NONE', *, *, #13454, .F. ) ;
#9953 = DIRECTION ( 'NONE',  ( 3.414809992136075319E-14, 0.5000000000047110094, 0.8660254037817188832 ) ) ;
#9954 = CARTESIAN_POINT ( 'NONE',  ( -0.7620000000000000107, -3544.061999999999898, 2239.771999999999935 ) ) ;
#9955 = PERSON_AND_ORGANIZATION_ROLE ( 'design_owner' ) ;
#9956 = VECTOR ( 'NONE', #11787, 1000.000000000000000 ) ;
#9957 = AXIS2_PLACEMENT_3D ( 'NONE', #13790, #880, #6303 ) ;
#9958 = CARTESIAN_POINT ( 'NONE',  ( 141.9245196256013060, -3581.268366753078681, 2248.906305629936924 ) ) ;
#9959 = ORIENTED_EDGE ( 'NONE', *, *, #16821, .F. ) ;
#9960 = DIRECTION ( 'NONE',  ( 0.000000000000000000, -1.000000000000000000, 0.000000000000000000 ) ) ;
#9961 = DATE_TIME_ROLE ( 'creation_date' ) ;
#9962 = EDGE_CURVE ( 'NONE', #15423, #14057, #2880, .T. ) ;
#9963 = DIRECTION ( 'NONE',  ( 1.000000000000000000, -2.334777064353000131E-14, -2.343004830739999973E-14 ) ) ;
#9964 = CARTESIAN_POINT ( 'NONE',  ( 67.10679999999999268, -3594.099999999999909, 2239.771999999999935 ) ) ;
#9965 = EDGE_CURVE ( 'NONE', #20114, #16063, #2070, .T. ) ;
#9966 = DIRECTION ( 'NONE',  ( 0.000000000000000000, 0.000000000000000000, 1.000000000000000000 ) ) ;
#9967 = VECTOR ( 'NONE', #7652, 1000.000000000000000 ) ;
#9968 = EDGE_CURVE ( 'NONE', #9781, #14341, #20848, .T. ) ;
#9969 = ORIENTED_EDGE ( 'NONE', *, *, #21014, .T. ) ;
#9970 = AXIS2_PLACEMENT_3D ( 'NONE', #6097, #13224, #20373 ) ;
#9971 = CIRCLE ( 'NONE', #11477, 4.114799999999974034 ) ;
#9972 = DIRECTION ( 'NONE',  ( 0.000000000000000000, 0.000000000000000000, 1.000000000000000000 ) ) ;
#9973 = VERTEX_POINT ( 'NONE', #3627 ) ;
#9974 = B_SPLINE_CURVE_WITH_KNOTS ( 'NONE', 3,
 ( #22124, #14764, #20156, #4324, #11464, #16847, #791, #4093, #7957, #15107 ),
 .UNSPECIFIED., .F., .F.,
 ( 4, 2, 1, 1, 2, 4 ),
 ( 0.000000000000000000, 0.06250000000027773617, 0.1250000000005554723, 0.2500000000010659806, 0.5000000000000244249, 1.000000000000000000 ),
 .UNSPECIFIED. ) ;
#9975 = ORIENTED_EDGE ( 'NONE', *, *, #19878, .T. ) ;
#9976 = CARTESIAN_POINT ( 'NONE',  ( 142.2400000000000091, -3694.430000000000291, 2255.774000000000342 ) ) ;
#9977 = VERTEX_POINT ( 'NONE', #21677 ) ;
#9978 = CARTESIAN_POINT ( 'NONE',  ( 144.7800000000000011, -3659.504999999999654, 2239.009999999999764 ) ) ;
#9979 = FACE_OUTER_BOUND ( 'NONE', #16180, .T. ) ;
#9980 = CIRCLE ( 'NONE', #23074, 2.844800000000091700 ) ;
#9981 = EDGE_CURVE ( 'NONE', #2446, #20779, #3739, .T. ) ;
#9982 = VERTEX_POINT ( 'NONE', #11011 ) ;
#9983 = TOROIDAL_SURFACE ( 'NONE', #7740, 4.114799999999999791, 1.270000000000000018 ) ;
#9984 = CARTESIAN_POINT ( 'NONE',  ( 12.69999999999999929, -3590.289999999999964, 2268.705139999999574 ) ) ;
#9985 =( LENGTH_UNIT ( ) NAMED_UNIT ( * ) SI_UNIT ( .MILLI., .METRE. ) );
#9986 = CARTESIAN_POINT ( 'NONE',  ( 117.9067999999989951, -3594.099999999999909, 2239.771999999999935 ) ) ;
#9987 = DIRECTION ( 'NONE',  ( 0.000000000000000000, 0.000000000000000000, 1.000000000000000000 ) ) ;
#9988 = PERSON_AND_ORGANIZATION_ROLE ( 'creator' ) ;
#9989 = AXIS2_PLACEMENT_3D ( 'NONE', #18337, #20217, #21518 ) ;
#9990 = DIRECTION ( 'NONE',  ( 0.000000000000000000, 0.000000000000000000, -1.000000000000000000 ) ) ;
#9991 = CARTESIAN_POINT ( 'NONE',  ( 139.6999999999999886, -3579.494999999999891, 2239.391000000000076 ) ) ;
#9992 = ORIENTED_EDGE ( 'NONE', *, *, #12507, .T. ) ;
#9993 = CARTESIAN_POINT ( 'NONE',  ( 116.8400000000000034, -3544.570000000000164, 2251.506800000000112 ) ) ;
#9994 = CARTESIAN_POINT ( 'NONE',  ( 141.9598072415896866, -3657.776943722216402, 2248.975963221890197 ) ) ;
#9995 = EDGE_CURVE ( 'NONE', #22409, #1396, #14304, .T. ) ;
#9996 = DIRECTION ( 'NONE',  ( 0.000000000000000000, 0.000000000000000000, -1.000000000000000000 ) ) ;
#9997 = EDGE_CURVE ( 'NONE', #2232, #17371, #17085, .T. ) ;
#9998 = ORIENTED_EDGE ( 'NONE', *, *, #20753, .T. ) ;
#9999 = CARTESIAN_POINT ( 'NONE',  ( 137.0230254594939368, -3543.701815209647521, 2255.430976451319566 ) ) ;
#10000 = CIRCLE ( 'NONE', #8895, 2.844799999998995244 ) ;
#10001 = ORIENTED_EDGE ( 'NONE', *, *, #10302, .T. ) ;
#10002 = EDGE_CURVE ( 'NONE', #15239, #12110, #1762, .T. ) ;
#10003 = VERTEX_POINT ( 'NONE', #5280 ) ;
#10004 = CARTESIAN_POINT ( 'NONE',  ( 12.69999999999999929, -3579.494999999999891, 2239.391000000000076 ) ) ;
#10005 = CIRCLE ( 'NONE', #17862, 2.844799999998995244 ) ;
#10006 = CYLINDRICAL_SURFACE ( 'NONE', #13650, 1.269999999999882334 ) ;
#10007 = CIRCLE ( 'NONE', #12263, 3.606800000000000228 ) ;
#10008 = ORIENTED_EDGE ( 'NONE', *, *, #1635, .F. ) ;
#10009 = ORIENTED_EDGE ( 'NONE', *, *, #19286, .T. ) ;
#10010 = CARTESIAN_POINT ( 'NONE',  ( 139.7000000000063835, -3576.802599999938593, 2239.391000000000076 ) ) ;
#10011 = PLANE ( 'NONE',  #20761 ) ;
#10012 = DIRECTION ( 'NONE',  ( -2.324635735433000053E-14, 2.336881798971000105E-14, -1.000000000000000000 ) ) ;
#10013 = ADVANCED_FACE ( 'NONE', ( #246 ), #1996, .F. ) ;
#10014 = VERTEX_POINT ( 'NONE', #16287 ) ;
#10015 = EDGE_CURVE ( 'NONE', #8026, #16063, #7757, .T. ) ;
#10016 = CARTESIAN_POINT ( 'NONE',  ( 12.69999999999999929, -3579.494999999999891, 2272.030000000000200 ) ) ;
#10017 = CARTESIAN_POINT ( 'NONE',  ( -6.349999999999999645, -3660.140000000000327, 2247.392000000000280 ) ) ;
#10018 = DIRECTION ( 'NONE',  ( 1.000000000000000000, -3.122111992759158343E-13, 0.000000000000000000 ) ) ;
#10019 = DIRECTION ( 'NONE',  ( 1.000000000000000000, -2.330758767201999921E-14, -2.339144844575000061E-14 ) ) ;
#10020 = ORIENTED_EDGE ( 'NONE', *, *, #1, .T. ) ;
#10021 = COORDINATED_UNIVERSAL_TIME_OFFSET ( 0, 0, .AHEAD. ) ;
#10022 = TOROIDAL_SURFACE ( 'NONE', #19377, 5.080000000000000071, 0.3810000000000000053 ) ;
#10023 = ORIENTED_EDGE ( 'NONE', *, *, #6018, .F. ) ;
#10024 = LINE ( 'NONE', #17165, #15025 ) ;
#10025 = CIRCLE ( 'NONE', #19381, 3.175000000000149925 ) ;
#10026 = CARTESIAN_POINT ( 'NONE',  ( 10.59475168835936998, -3581.408331351744437, 2248.656493541727286 ) ) ;
#10027 = DIRECTION ( 'NONE',  ( -1.000000000000000000, 0.000000000000000000, 0.000000000000000000 ) ) ;
#10028 = ORIENTED_EDGE ( 'NONE', *, *, #20683, .F. ) ;
#10029 = FACE_BOUND ( 'NONE', #2014, .T. ) ;
#10030 = CARTESIAN_POINT ( 'NONE',  ( 35.56000000000000227, -3670.300000000000182, 2250.236800000000130 ) ) ;
#10031 = CARTESIAN_POINT ( 'NONE',  ( 145.1668838676556561, -3661.170433021055032, 2244.740127772376582 ) ) ;
#10032 = ORIENTED_EDGE ( 'NONE', *, *, #18982, .T. ) ;
#10033 = CARTESIAN_POINT ( 'NONE',  ( 12.69999999999999929, -3579.494999999999891, 2255.774000000000342 ) ) ;
#10034 = CARTESIAN_POINT ( 'NONE',  ( 14.85464569033375781, -3661.362555271571637, 2249.960724679396208 ) ) ;
#10035 = DIRECTION ( 'NONE',  ( 1.000000000000000000, 5.432398939370943590E-28, -2.324635735433000369E-14 ) ) ;
#10036 = ORIENTED_EDGE ( 'NONE', *, *, #16521, .F. ) ;
#10037 = DIRECTION ( 'NONE',  ( 0.000000000000000000, 0.000000000000000000, -1.000000000000000000 ) ) ;
#10038 = CARTESIAN_POINT ( 'NONE',  ( 20.32000000000000028, -3544.061999999999898, 2292.819899999999961 ) ) ;
#10039 = CARTESIAN_POINT ( 'NONE',  ( 11.76748838596000013, -3596.803600169999754, 2279.779819357000179 ) ) ;
#10040 = LINE ( 'NONE', #13563, #11670 ) ;
#10041 = ORIENTED_EDGE ( 'NONE', *, *, #2987, .T. ) ;
#10042 = ORIENTED_EDGE ( 'NONE', *, *, #16554, .T. ) ;
#10043 = ORIENTED_EDGE ( 'NONE', *, *, #76, .F. ) ;
#10044 = DIRECTION ( 'NONE',  ( 0.000000000000000000, -1.000000000000000000, 0.000000000000000000 ) ) ;
#10045 = ORIENTED_EDGE ( 'NONE', *, *, #18836, .T. ) ;
#10046 = CARTESIAN_POINT ( 'NONE',  ( 142.5262150954257834, -3659.130943335864686, 2257.957974173014918 ) ) ;
#10047 = APPROVAL_ROLE ( '' ) ;
#10048 = CARTESIAN_POINT ( 'NONE',  ( 117.1447999999989946, -3644.899999999999636, 2259.837999999999738 ) ) ;
#10049 = CARTESIAN_POINT ( 'NONE',  ( 9.904004635912999177, -3660.053455317999578, 2257.950092655999924 ) ) ;
#10050 = AXIS2_PLACEMENT_3D ( 'NONE', #11228, #4532, #11671 ) ;
#10051 = CARTESIAN_POINT ( 'NONE',  ( 15.54479972196000048, -3659.413078500999745, 2257.962943248000101 ) ) ;
#10052 = APPLIED_PERSON_AND_ORGANIZATION_ASSIGNMENT ( #8820, #3763, ( #15546 ) ) ;
#10053 = DIRECTION ( 'NONE',  ( 1.000000000000000000, -0.000000000000000000, 1.224646799147353207E-16 ) ) ;
#10054 = CARTESIAN_POINT ( 'NONE',  ( 136.9269754645999910, -3578.860002036999958, 2250.236803302000226 ) ) ;
#10055 = ORIENTED_EDGE ( 'NONE', *, *, #5146, .T. ) ;
#10056 = CARTESIAN_POINT ( 'NONE',  ( 136.8552000000009912, -3659.504999999999654, 2257.962944264955240 ) ) ;
#10057 = EDGE_CURVE ( 'NONE', #5906, #9973, #14868, .T. ) ;
#10058 = DIRECTION ( 'NONE',  ( 1.000000000000000000, 0.000000000000000000, 0.000000000000000000 ) ) ;
#10059 = VERTEX_POINT ( 'NONE', #10664 ) ;
#10060 = ADVANCED_FACE ( 'NONE', ( #19573 ), #2116, .T. ) ;
#10061 = DIRECTION ( 'NONE',  ( 0.7249994335945011414, 6.337882393832011514E-14, 0.6887494619146010688 ) ) ;
#10062 = SPHERICAL_SURFACE ( 'NONE', #22948, 0.7620000000000000107 ) ;
#10063 = EDGE_CURVE ( 'NONE', #15557, #952, #7387, .T. ) ;
#10064 = ORIENTED_EDGE ( 'NONE', *, *, #631, .F. ) ;
#10065 = ORIENTED_EDGE ( 'NONE', *, *, #16169, .F. ) ;
#10066 = CARTESIAN_POINT ( 'NONE',  ( 134.2797385147190710, -3581.306672009827707, 2245.940466658847981 ) ) ;
#10067 = ORIENTED_EDGE ( 'NONE', *, *, #21289, .T. ) ;
#10068 = CARTESIAN_POINT ( 'NONE',  ( 139.6999999999999886, -3659.504999999999654, 2239.391000000000076 ) ) ;
#10069 = DIRECTION ( 'NONE',  ( -1.000000000000000000, 0.000000000000000000, 0.000000000000000000 ) ) ;
#10070 = EDGE_CURVE ( 'NONE', #15388, #7817, #7016, .T. ) ;
#10071 = CARTESIAN_POINT ( 'NONE',  ( 142.3965585763085642, -3580.405385417485377, 2249.782477816118899 ) ) ;
#10072 = VERTEX_POINT ( 'NONE', #19923 ) ;
#10073 = CARTESIAN_POINT ( 'NONE',  ( 139.3249801397857652, -3582.321213456867099, 2257.597441011073897 ) ) ;
#10074 = APPLICATION_PROTOCOL_DEFINITION ( 'international standard', 'automotive_design', 2000, #1993 ) ;
#10075 = DIRECTION ( 'NONE',  ( -1.000000000000000000, 0.000000000000000000, 0.000000000000000000 ) ) ;
#10076 = CARTESIAN_POINT ( 'NONE',  ( 14.62656071289291404, -3581.588169671847027, 2248.198601268956281 ) ) ;
#10077 = AXIS2_PLACEMENT_3D ( 'NONE', #23019, #3228, #14249 ) ;
#10078 = CARTESIAN_POINT ( 'NONE',  ( 134.2752418639106509, -3657.706857388223852, 2245.917987683012143 ) ) ;
#10079 = APPLIED_APPROVAL_ASSIGNMENT ( #21811, ( #17188 ) ) ;
#10080 = VERTEX_POINT ( 'NONE', #21572 ) ;
#10081 = AXIS2_PLACEMENT_3D ( 'NONE', #10244, #2743, #9887 ) ;
#10082 = CARTESIAN_POINT ( 'NONE',  ( 142.4066795037432485, -3660.429743292840158, 2250.236799901205814 ) ) ;
#10083 =( REPRESENTATION_RELATIONSHIP ('NONE','NONE', #20448, #1421 ) REPRESENTATION_RELATIONSHIP_WITH_TRANSFORMATION ( #19541 )SHAPE_REPRESENTATION_RELATIONSHIP( ) );
#10084 = EDGE_CURVE ( 'NONE', #19890, #22201, #9980, .T. ) ;
#10085 = CYLINDRICAL_SURFACE ( 'NONE', #14416, 0.3810000000000260956 ) ;
#10086 = ORIENTED_EDGE ( 'NONE', *, *, #17971, .F. ) ;
#10087 = DIRECTION ( 'NONE',  ( 1.000000000000000000, 0.000000000000000000, 0.000000000000000000 ) ) ;
#10088 = ADVANCED_FACE ( 'NONE', ( #5526 ), #19807, .T. ) ;
#10089 = ADVANCED_FACE ( 'NONE', ( #10896 ), #12769, .T. ) ;
#10090 = DIRECTION ( 'NONE',  ( 6.119339505807659940E-14, -1.000000000000000000, 0.000000000000000000 ) ) ;
#10091 = ORIENTED_EDGE ( 'NONE', *, *, #11994, .F. ) ;
#10092 = ORIENTED_EDGE ( 'NONE', *, *, #19838, .T. ) ;
#10093 = DIRECTION ( 'NONE',  ( 0.000000000000000000, 1.000000000000000000, 0.000000000000000000 ) ) ;
#10094 = FACE_OUTER_BOUND ( 'NONE', #20329, .T. ) ;
#10095 = CIRCLE ( 'NONE', #17201, 0.7619999999999294005 ) ;
#10096 = VERTEX_POINT ( 'NONE', #14652 ) ;
#10097 = LINE ( 'NONE', #20123, #19943 ) ;
#10098 = FACE_OUTER_BOUND ( 'NONE', #18381, .T. ) ;
#10099 = CARTESIAN_POINT ( 'NONE',  ( 12.69998491500954962, -3642.347301254179911, 2279.817638609000369 ) ) ;
#10100 = PRODUCT_DEFINITION_FORMATION_WITH_SPECIFIED_SOURCE ( 'ANY', '', #11987, .NOT_KNOWN. ) ;
#10101 = AXIS2_PLACEMENT_3D ( 'NONE', #20738, #17330, #4686 ) ;
#10102 = CARTESIAN_POINT ( 'NONE',  ( 9.209369265467998389, -3543.299999999999727, 2282.113800000000083 ) ) ;
#10103 = PERSON_AND_ORGANIZATION ( #5446, #1895 ) ;
#10104 = LINE ( 'NONE', #1551, #20804 ) ;
#10105 = CYLINDRICAL_SURFACE ( 'NONE', #4927, 3.175000000000149925 ) ;
#10106 = PLANE ( 'NONE',  #6681 ) ;
#10107 = ADVANCED_FACE ( 'NONE', ( #21791, #5755 ), #12886, .F. ) ;
#10108 = PRODUCT ( 'Screw 7', 'Screw 7', '', ( #5836 ) ) ;
#10109 = DIRECTION ( 'NONE',  ( 0.000000000000000000, 0.000000000000000000, 1.000000000000000000 ) ) ;
#10110 = ORIENTED_EDGE ( 'NONE', *, *, #11208, .F. ) ;
#10111 = CARTESIAN_POINT ( 'NONE',  ( 137.1599999999999966, -3544.570000000000164, 2255.774000000000342 ) ) ;
#10112 = CIRCLE ( 'NONE', #18350, 2.844799999999999773 ) ;
#10113 = EDGE_CURVE ( 'NONE', #15883, #2915, #581, .T. ) ;
#10114 = LOCAL_TIME ( 17, 37, 43.00000000000000000, #9481 ) ;
#10115 = APPROVAL_PERSON_ORGANIZATION ( #8671, #889, #12852 ) ;
#10116 = ORIENTED_EDGE ( 'NONE', *, *, #2100, .T. ) ;
#10117 = CARTESIAN_POINT ( 'NONE',  ( 4.770976268947110022, -3695.599092773176380, 2259.826110292242447 ) ) ;
#10118 = DIRECTION ( 'NONE',  ( 0.000000000000000000, 1.000000000000000000, 0.000000000000000000 ) ) ;
#10119 = ORIENTED_EDGE ( 'NONE', *, *, #17963, .F. ) ;
#10120 = EDGE_LOOP ( 'NONE', ( #8684, #2589, #14124, #14665, #8494, #8444, #8986 ) ) ;
#10121 = CARTESIAN_POINT ( 'NONE',  ( 76.20000000000000284, -3670.300000000000182, 2259.837999999999738 ) ) ;
#10122 = CARTESIAN_POINT ( 'NONE',  ( 142.2400000000000091, -3544.570000000000164, 2255.774000000000342 ) ) ;
#10123 = CARTESIAN_POINT ( 'NONE',  ( 19.05000000000000071, -3582.035000000000309, 2247.392000000000280 ) ) ;
#10124 = ADVANCED_FACE ( 'NONE', ( #4094 ), #2110, .T. ) ;
#10125 = ORIENTED_EDGE ( 'NONE', *, *, #5725, .F. ) ;
#10126 = ADVANCED_FACE ( 'NONE', ( #6094 ), #11684, .F. ) ;
#10127 = CARTESIAN_POINT ( 'NONE',  ( 130.6067999999989979, -3568.700000000000273, 2239.009999999999764 ) ) ;
#10128 = CARTESIAN_POINT ( 'NONE',  ( 15.18950216430036981, -3638.065185255141387, 2296.591799999884188 ) ) ;
#10129 = DIRECTION ( 'NONE',  ( 1.000000000000000000, 0.000000000000000000, 0.000000000000000000 ) ) ;
#10130 = DIRECTION ( 'NONE',  ( -1.000000000000000000, 0.000000000000000000, 0.000000000000000000 ) ) ;
#10131 = CARTESIAN_POINT ( 'NONE',  ( 20.60962197524936457, -3695.579402567507259, 2259.874448544494044 ) ) ;
#10132 = ORIENTED_EDGE ( 'NONE', *, *, #1364, .T. ) ;
#10133 = DATE_AND_TIME ( #1106, #16137 ) ;
#10134 = VERTEX_POINT ( 'NONE', #904 ) ;
#10135 = LINE ( 'NONE', #13539, #12021 ) ;
#10136 = SECURITY_CLASSIFICATION ( '', '', #209 ) ;
#10137 = EDGE_CURVE ( 'NONE', #3108, #11298, #926, .T. ) ;
#10138 = PRODUCT_DEFINITION_FORMATION_WITH_SPECIFIED_SOURCE ( 'ANY', '', #21176, .NOT_KNOWN. ) ;
#10139 = DIRECTION ( 'NONE',  ( -1.000000000000000000, 0.000000000000000000, 0.000000000000000000 ) ) ;
#10140 = FACE_BOUND ( 'NONE', #6988, .T. ) ;
#10141 = VERTEX_POINT ( 'NONE', #13344 ) ;
#10142 = VECTOR ( 'NONE', #2423, 1000.000000000000000 ) ;
#10143 = EDGE_CURVE ( 'NONE', #12177, #8402, #11808, .T. ) ;
#10144 = CARTESIAN_POINT ( 'NONE',  ( -0.7620000000000000107, -3578.860000000000127, 2247.392000000000280 ) ) ;
#10145 = EDGE_CURVE ( 'NONE', #17805, #16889, #16677, .T. ) ;
#10146 = DIRECTION ( 'NONE',  ( 0.000000000000000000, 0.000000000000000000, 1.000000000000000000 ) ) ;
#10147 = CARTESIAN_POINT ( 'NONE',  ( 145.1120077101980712, -3661.341326264781856, 2244.812092251788727 ) ) ;
#10148 = CARTESIAN_POINT ( 'NONE',  ( 57.14999999999999858, -3568.700000000000273, 2247.392000000000280 ) ) ;
#10149 = CARTESIAN_POINT ( 'NONE',  ( 11.74244832569119623, -3662.185093235403201, 2249.370122485771844 ) ) ;
#10150 = CARTESIAN_POINT ( 'NONE',  ( 79.04479999999999507, -3568.700000000000273, 2239.771999999999935 ) ) ;
#10151 = ORIENTED_EDGE ( 'NONE', *, *, #3051, .T. ) ;
#10152 = DIRECTION ( 'NONE',  ( -1.000000000000000000, 0.000000000000000000, 0.000000000000000000 ) ) ;
#10153 = CARTESIAN_POINT ( 'NONE',  ( 10.36831320283000046, -3640.848700000000008, 2296.210799999999836 ) ) ;
#10154 = EDGE_CURVE ( 'NONE', #15928, #22036, #17544, .T. ) ;
#10155 = DIRECTION ( 'NONE',  ( 0.000000000000000000, 0.000000000000000000, -1.000000000000000000 ) ) ;
#10156 = DIRECTION ( 'NONE',  ( 0.000000000000000000, 0.000000000000000000, -1.000000000000000000 ) ) ;
#10157 = DIRECTION ( 'NONE',  ( 0.000000000000000000, 0.000000000000000000, -1.000000000000000000 ) ) ;
#10158 = VERTEX_POINT ( 'NONE', #3022 ) ;
#10159 = AXIS2_PLACEMENT_3D ( 'NONE', #8990, #16141, #14274 ) ;
#10160 = ORIENTED_EDGE ( 'NONE', *, *, #6510, .T. ) ;
#10161 = VECTOR ( 'NONE', #2832, 1000.000000000000000 ) ;
#10162 = FACE_OUTER_BOUND ( 'NONE', #6177, .T. ) ;
#10163 = ORIENTED_EDGE ( 'NONE', *, *, #13381, .T. ) ;
#10164 = CARTESIAN_POINT ( 'NONE',  ( 9.916876041047901325, -3543.482543405149954, 2255.165366398012793 ) ) ;
#10165 = DIRECTION ( 'NONE',  ( 0.000000000000000000, 0.000000000000000000, 1.000000000000000000 ) ) ;
#10166 = ORIENTED_EDGE ( 'NONE', *, *, #19404, .F. ) ;
#10167 = DIRECTION ( 'NONE',  ( 0.000000000000000000, 0.000000000000000000, -1.000000000000000000 ) ) ;
#10168 = DIRECTION ( 'NONE',  ( 0.000000000000000000, 1.000000000000000000, 1.224646799147353207E-16 ) ) ;
#10169 = CYLINDRICAL_SURFACE ( 'NONE', #16714, 2.844799999999009010 ) ;
#10170 = DIRECTION ( 'NONE',  ( 0.000000000000000000, 0.000000000000000000, -1.000000000000000000 ) ) ;
#10171 = PLANE ( 'NONE',  #14014 ) ;
#10172 = EDGE_LOOP ( 'NONE', ( #17107, #6074, #5151, #18176 ) ) ;
#10173 = AXIS2_PLACEMENT_3D ( 'NONE', #17019, #2846, #1193 ) ;
#10174 = FACE_OUTER_BOUND ( 'NONE', #1425, .T. ) ;
#10175 = VECTOR ( 'NONE', #13829, 1000.000000000000000 ) ;
#10176 = DIRECTION ( 'NONE',  ( 0.000000000000000000, -2.336881798971000105E-14, -1.000000000000000000 ) ) ;
#10177 = ORIENTED_EDGE ( 'NONE', *, *, #7583, .T. ) ;
#10178 = CARTESIAN_POINT ( 'NONE',  ( 10.36831320284000135, -3638.156300000000101, 2296.210799999999836 ) ) ;
#10179 = DIRECTION ( 'NONE',  ( 0.000000000000000000, 1.000000000000000000, 0.000000000000000000 ) ) ;
#10180 = ORIENTED_EDGE ( 'NONE', *, *, #21483, .F. ) ;
#10181 = ORIENTED_EDGE ( 'NONE', *, *, #14636, .F. ) ;
#10182 = CARTESIAN_POINT ( 'NONE',  ( 139.7000000000068383, -3656.630370510378725, 2239.010000000095715 ) ) ;
#10183 = PRODUCT_DEFINITION_CONTEXT ( 'detailed design', #21162, 'design' ) ;
#10184 = ORIENTED_EDGE ( 'NONE', *, *, #6233, .F. ) ;
#10185 = VECTOR ( 'NONE', #4178, 1000.000000000000000 ) ;
#10186 = VERTEX_POINT ( 'NONE', #20715 ) ;
#10187 = DIRECTION ( 'NONE',  ( 0.000000000000000000, 0.000000000000000000, 1.000000000000000000 ) ) ;
#10188 = DIRECTION ( 'NONE',  ( 0.000000000000000000, 0.000000000000000000, 1.000000000000000000 ) ) ;
#10189 = DIRECTION ( 'NONE',  ( 0.7249994335945011414, 0.000000000000000000, 0.6887494619146010688 ) ) ;
#10190 = TOROIDAL_SURFACE ( 'NONE', #1199, 3.606799999998999695, 0.7620000000000000107 ) ;
#10191 = ORIENTED_EDGE ( 'NONE', *, *, #13984, .T. ) ;
#10193 = CARTESIAN_POINT ( 'NONE',  ( 136.8552000000009912, -3579.494999999999891, 2257.962944264955695 ) ) ;
#10192 = CIRCLE ( 'NONE', #19925, 4.114799999999974034 ) ;
#10194 = PERSON_AND_ORGANIZATION_ROLE ( 'classification_officer' ) ;
#10195 = CIRCLE ( 'NONE', #2343, 2.844800000000001550 ) ;
#10196 = EDGE_CURVE ( 'NONE', #12925, #13091, #11812, .T. ) ;
#10197 = DIRECTION ( 'NONE',  ( -0.000000000000000000, -1.000000000000000000, -0.000000000000000000 ) ) ;
#10198 = CARTESIAN_POINT ( 'NONE',  ( 14.56067386347176651, -3581.648071076505403, 2246.799892842011559 ) ) ;
#10199 = CARTESIAN_POINT ( 'NONE',  ( 134.1386338306796802, -3658.188830379587216, 2245.321775082328259 ) ) ;
#10200 = PERSON ( 'NAUO-PER10', 'UNSPECIFIED', 'UNSPECIFIED', ('UNSPECIFIED'), ('UNSPECIFIED'), ('UNSPECIFIED') ) ;
#10201 = EDGE_LOOP ( 'NONE', ( #14060, #15783, #19384, #668 ) ) ;
#10202 = CIRCLE ( 'NONE', #19196, 0.7620000000000126672 ) ;
#10203 = CARTESIAN_POINT ( 'NONE',  ( 15.24000000000000021, -3694.746619018625552, 2255.774000000000342 ) ) ;
#10204 = CARTESIAN_POINT ( 'NONE',  ( 142.0316867971391446, -3658.158799999964231, 2239.391000000000076 ) ) ;
#10205 = ORIENTED_EDGE ( 'NONE', *, *, #9842, .F. ) ;
#10206 = DIRECTION ( 'NONE',  ( 0.000000000000000000, -1.000000000000000000, 0.000000000000000000 ) ) ;
#10207 = TOROIDAL_SURFACE ( 'NONE', #17313, 3.606799999998999695, 0.7620000000000000107 ) ;
#10208 = VECTOR ( 'NONE', #3528, 1000.000000000000000 ) ;
#10209 = CARTESIAN_POINT ( 'NONE',  ( 20.32000000000000028, -3568.700000000000273, 2289.213099999999940 ) ) ;
#10210 = ORIENTED_EDGE ( 'NONE', *, *, #14723, .F. ) ;
#10211 = CARTESIAN_POINT ( 'NONE',  ( 20.43202024788000060, -3544.321224513000288, 2260.577432830999896 ) ) ;
#10212 = DIRECTION ( 'NONE',  ( 0.000000000000000000, 0.000000000000000000, -1.000000000000000000 ) ) ;
#10213 = ORIENTED_EDGE ( 'NONE', *, *, #19514, .F. ) ;
#10214 = APPLIED_PERSON_AND_ORGANIZATION_ASSIGNMENT ( #6751, #22548, ( #18354 ) ) ;
#10215 = DIRECTION ( 'NONE',  ( 1.000000000000000000, 0.000000000000000000, 0.000000000000000000 ) ) ;
#10216 = CARTESIAN_POINT ( 'NONE',  ( 15.53879320304153744, -3659.720045446122185, 2250.207625598751747 ) ) ;
#10217 = SHAPE_REPRESENTATION_RELATIONSHIP ( 'NONE' , 'NONE' ,  #3816, #12702 ) ;
#10218 = LINE ( 'NONE', #17353, #17666 ) ;
#10219 = CARTESIAN_POINT ( 'NONE',  ( 136.8842289382999979, -3579.071024516000307, 2250.231635222000023 ) ) ;
#10220 = AXIS2_PLACEMENT_3D ( 'NONE', #16851, #7963, #5757 ) ;
#10221 = COORDINATED_UNIVERSAL_TIME_OFFSET ( 0, 0, .AHEAD. ) ;
#10222 = EDGE_CURVE ( 'NONE', #3845, #10958, #4701, .T. ) ;
#10223 = DIRECTION ( 'NONE',  ( 0.000000000000000000, 0.000000000000000000, 1.000000000000000000 ) ) ;
#10224 = CARTESIAN_POINT ( 'NONE',  ( 95.25000000000000000, -3543.300000000000182, 2243.277199999999993 ) ) ;
#10226 = EDGE_CURVE ( 'NONE', #17073, #3671, #16322, .T. ) ;
#10225 = DIRECTION ( 'NONE',  ( -0.5000000000031612490, -0.8660254037826135010, 0.000000000000000000 ) ) ;
#10227 = AXIS2_PLACEMENT_3D ( 'NONE', #20643, #15043, #11739 ) ;
#10228 = ADVANCED_FACE ( 'NONE', ( #22706 ), #20841, .F. ) ;
#10229 = AXIS2_PLACEMENT_3D ( 'NONE', #19468, #6939, #10325 ) ;
#10230 = CARTESIAN_POINT ( 'NONE',  ( 141.5168167239393711, -3657.315756010447785, 2247.770112268088724 ) ) ;
#10231 = ORIENTED_EDGE ( 'NONE', *, *, #20299, .F. ) ;
#10232 = LINE ( 'NONE', #10702, #17075 ) ;
#10233 = ORIENTED_EDGE ( 'NONE', *, *, #5271, .F. ) ;
#10234 = CIRCLE ( 'NONE', #22939, 2.844799999999961582 ) ;
#10235 = CARTESIAN_POINT ( 'NONE',  ( 12.69999999999999929, -3579.494999999999891, 2239.391000000000076 ) ) ;
#10236 = ORIENTED_EDGE ( 'NONE', *, *, #10145, .T. ) ;
#10237 = VERTEX_POINT ( 'NONE', #18968 ) ;
#10238 = SPHERICAL_SURFACE ( 'NONE', #9409, 1.270000000000000018 ) ;
#10239 = EDGE_CURVE ( 'NONE', #15577, #17007, #22466, .T. ) ;
#10240 = CARTESIAN_POINT ( 'NONE',  ( 151.4000000000000057, -3694.430000000000291, 2239.039032635400417 ) ) ;
#10241 = DIRECTION ( 'NONE',  ( -1.224646799147353207E-16, 1.000000000000000000, 0.000000000000000000 ) ) ;
#10242 = VERTEX_POINT ( 'NONE', #10404 ) ;
#10243 = CARTESIAN_POINT ( 'NONE',  ( 139.6999999999999886, -3659.504999999999654, 2239.391000000000076 ) ) ;
#10244 = CARTESIAN_POINT ( 'NONE',  ( 12.69999999999999929, -3585.971999999999753, 2268.705139999999574 ) ) ;
#10245 = FACE_OUTER_BOUND ( 'NONE', #16580, .T. ) ;
#10246 = DIRECTION ( 'NONE',  ( 0.000000000000000000, -1.000000000000000000, 0.000000000000000000 ) ) ;
#10247 = CARTESIAN_POINT ( 'NONE',  ( 12.69999999999999929, -3656.329999999999472, 2245.359999999999673 ) ) ;
#10248 = ORIENTED_EDGE ( 'NONE', *, *, #15852, .T. ) ;
#10249 = APPLICATION_PROTOCOL_DEFINITION ( 'international standard', 'automotive_design', 2000, #18003 ) ;
#10250 = ORIENTED_EDGE ( 'NONE', *, *, #20380, .F. ) ;
#10251 = CARTESIAN_POINT ( 'NONE',  ( 19.05000000000000071, -3660.140000000000327, 2247.392000000000280 ) ) ;
#10252 = AXIS2_PLACEMENT_3D ( 'NONE', #2792, #4546, #9936 ) ;
#10253 = ADVANCED_FACE ( 'NONE', ( #13814 ), #4661, .T. ) ;
#10254 = CARTESIAN_POINT ( 'NONE',  ( 10.51600127293235154, -3581.318391123547372, 2248.824551120855176 ) ) ;
#10255 = SPHERICAL_SURFACE ( 'NONE', #16081, 0.7620000000000000107 ) ;
#10256 = VECTOR ( 'NONE', #863, 999.9999999999998863 ) ;
#10257 = ORIENTED_EDGE ( 'NONE', *, *, #10523, .T. ) ;
#10258 = CARTESIAN_POINT ( 'NONE',  ( 101.5999999999999943, -3568.700000000000273, 2259.837999999999738 ) ) ;
#10259 = EDGE_CURVE ( 'NONE', #7810, #22994, #15798, .T. ) ;
#10260 = EDGE_CURVE ( 'NONE', #16631, #2427, #21198, .T. ) ;
#10261 = DIRECTION ( 'NONE',  ( 1.000000000000000000, 0.000000000000000000, 0.000000000000000000 ) ) ;
#10262 = DIRECTION ( 'NONE',  ( 2.336881798971000105E-14, 2.336881798971000105E-14, 1.000000000000000000 ) ) ;
#10263 = DIRECTION ( 'NONE',  ( 0.000000000000000000, 0.000000000000000000, -1.000000000000000000 ) ) ;
#10264 = CARTESIAN_POINT ( 'NONE',  ( 10.44172237351025245, -3661.244228531198132, 2250.017997341298724 ) ) ;
#10265 = CARTESIAN_POINT ( 'NONE',  ( 147.4602386003344918, -3543.693183278424385, 2260.248803182081247 ) ) ;
#10266 = ORIENTED_EDGE ( 'NONE', *, *, #10653, .T. ) ;
#10267 = ADVANCED_FACE ( 'NONE', ( #3369, #10522 ), #6553, .T. ) ;
#10268 = CARTESIAN_POINT ( 'NONE',  ( 55.57575231171000496, -3695.699999999999818, 2275.763800000000174 ) ) ;
#10269 = CIRCLE ( 'NONE', #8404, 1.269999999999882334 ) ;
#10270 = CARTESIAN_POINT ( 'NONE',  ( 105.2067999999999870, -3670.300000000000182, 2260.600000000000364 ) ) ;
#10271 = VECTOR ( 'NONE', #12724, 1000.000000000000000 ) ;
#10272 = CARTESIAN_POINT ( 'NONE',  ( 136.9269649396999853, -3660.140004248000423, 2250.236800000000130 ) ) ;
#10273 = VECTOR ( 'NONE', #15758, 1000.000000000000000 ) ;
#10274 = CARTESIAN_POINT ( 'NONE',  ( 14.57276727744440237, -3657.363329750993216, 2248.017389562041444 ) ) ;
#10275 = CARTESIAN_POINT ( 'NONE',  ( 15.54479970632153751, -3579.286029448822319, 2250.212875600666393 ) ) ;
#10276 = ORIENTED_EDGE ( 'NONE', *, *, #16148, .F. ) ;
#10277 = EDGE_CURVE ( 'NONE', #2318, #5890, #12575, .T. ) ;
#10278 = VERTEX_POINT ( 'NONE', #1852 ) ;
#10279 = DIRECTION ( 'NONE',  ( -1.000000000000000000, 0.000000000000000000, 0.000000000000000000 ) ) ;
#10280 = ORIENTED_EDGE ( 'NONE', *, *, #1779, .T. ) ;
#10281 = CARTESIAN_POINT ( 'NONE',  ( 14.90539642439000012, -3581.299404879999656, 2257.813168336999752 ) ) ;
#10282 = CONTEXT_DEPENDENT_SHAPE_REPRESENTATION ( #12938, #11270 ) ;
#10283 = CARTESIAN_POINT ( 'NONE',  ( 38.10000000000000142, -3644.899999999999636, 2259.837999999999738 ) ) ;
#10284 = CARTESIAN_POINT ( 'NONE',  ( 3.048000000000000043, -3544.061999999999898, 2229.612000000000080 ) ) ;
#10285 = CARTESIAN_POINT ( 'NONE',  ( 9.970491213060000746, -3660.322548418000224, 2257.932969814999979 ) ) ;
#10286 = CIRCLE ( 'NONE', #22248, 5.714999999999999858 ) ;
#10287 = TOROIDAL_SURFACE ( 'NONE', #196, 3.606799999998999695, 0.7620000000000000107 ) ;
#10288 = CARTESIAN_POINT ( 'NONE',  ( 63.50000000000000000, -3594.099999999999909, 2259.837999999999738 ) ) ;
#10289 = CIRCLE ( 'NONE', #198, 0.7619999999999294005 ) ;
#10290 = CARTESIAN_POINT ( 'NONE',  ( 12.69999999999999929, -3659.504999999999654, 2246.630000000000109 ) ) ;
#10291 = EDGE_CURVE ( 'NONE', #825, #4416, #12513, .T. ) ;
#10292 = AXIS2_PLACEMENT_3D ( 'NONE', #17124, #13617, #4822 ) ;
#10293 = DIRECTION ( 'NONE',  ( 0.000000000000000000, 0.000000000000000000, 1.000000000000000000 ) ) ;
#10294 = ORIENTED_EDGE ( 'NONE', *, *, #10196, .F. ) ;
#10295 = FACE_OUTER_BOUND ( 'NONE', #299, .T. ) ;
#10296 = CARTESIAN_POINT ( 'NONE',  ( -12.69999999999999929, -3661.706170453011509, 2250.104686796980332 ) ) ;
#10297 = VERTEX_POINT ( 'NONE', #10633 ) ;
#10298 = LINE ( 'NONE', #1502, #9182 ) ;
#10299 = CARTESIAN_POINT ( 'NONE',  ( 10.33664877816801564, -3657.921536567248950, 2249.173046712553969 ) ) ;
#10300 = ORIENTED_EDGE ( 'NONE', *, *, #20722, .T. ) ;
#10301 = VECTOR ( 'NONE', #163, 1000.000000000000000 ) ;
#10302 = EDGE_CURVE ( 'NONE', #5168, #16435, #12146, .T. ) ;
#10303 = AXIS2_PLACEMENT_3D ( 'NONE', #6103, #11938, #13229 ) ;
#10304 = EDGE_CURVE ( 'NONE', #4174, #14745, #4340, .T. ) ;
#10305 = ORIENTED_EDGE ( 'NONE', *, *, #1850, .T. ) ;
#10306 = AXIS2_PLACEMENT_3D ( 'NONE', #9583, #11450, #6191 ) ;
#10307 = LINE ( 'NONE', #15818, #3224 ) ;
#10308 = PERSON_AND_ORGANIZATION_ROLE ( 'design_supplier' ) ;
#10309 = CIRCLE ( 'NONE', #222, 2.844800000000091700 ) ;
#10310 = CYLINDRICAL_SURFACE ( 'NONE', #22945, 1.269999999999882334 ) ;
#10311 = ORIENTED_EDGE ( 'NONE', *, *, #1416, .T. ) ;
#10312 = CARTESIAN_POINT ( 'NONE',  ( 131.7409145027432658, -3695.628299765889096, 2259.750699691084264 ) ) ;
#10313 = VECTOR ( 'NONE', #6591, 1000.000000000000000 ) ;
#10314 = PERSON_AND_ORGANIZATION ( #5446, #1895 ) ;
#10315 = LINE ( 'NONE', #4925, #4394 ) ;
#10316 = CARTESIAN_POINT ( 'NONE',  ( 14.53546583297210937, -3581.668498076454853, 2247.847147041044082 ) ) ;
#10317 = CARTESIAN_POINT ( 'NONE',  ( 134.1464163013289408, -3658.155994145996374, 2245.352780909838657 ) ) ;
#10318 = CIRCLE ( 'NONE', #15192, 3.606799999998994366 ) ;
#10319 = CARTESIAN_POINT ( 'NONE',  ( 144.7800000000000011, -3579.494999999999891, 2244.978999999999814 ) ) ;
#10320 = VERTEX_POINT ( 'NONE', #1969 ) ;
#10321 = VECTOR ( 'NONE', #11663, 1000.000000000000000 ) ;
#10322 = LINE ( 'NONE', #1528, #20063 ) ;
#10323 = LINE ( 'NONE', #17698, #2072 ) ;
#10324 = ORIENTED_EDGE ( 'NONE', *, *, #3117, .F. ) ;
#10325 = DIRECTION ( 'NONE',  ( 1.000000000000000000, 0.000000000000000000, 0.000000000000000000 ) ) ;
#10326 = ORIENTED_EDGE ( 'NONE', *, *, #4555, .T. ) ;
#10327 = VECTOR ( 'NONE', #9501, 1000.000000000000000 ) ;
#10328 = EDGE_LOOP ( 'NONE', ( #20417, #1792, #18331, #11539, #3494 ) ) ;
#10329 = AXIS2_PLACEMENT_3D ( 'NONE', #14094, #19477, #19129 ) ;
#10330 = ORIENTED_EDGE ( 'NONE', *, *, #21718, .F. ) ;
#10331 = CARTESIAN_POINT ( 'NONE',  ( 20.37131517211999920, -3544.241664856000170, 2260.557504477000293 ) ) ;
#10332 = CARTESIAN_POINT ( 'NONE',  ( 134.0204252830999962, -3660.140268639000169, 2244.547525601999951 ) ) ;
#10333 = ORIENTED_EDGE ( 'NONE', *, *, #4079, .F. ) ;
#10334 = DIRECTION ( 'NONE',  ( 0.000000000000000000, 0.000000000000000000, -1.000000000000000000 ) ) ;
#10335 = CARTESIAN_POINT ( 'NONE',  ( 10.36831320284000135, -3598.151299999999992, 2292.781800000000203 ) ) ;
#10336 = CARTESIAN_POINT ( 'NONE',  ( 12.69999999999999929, -3642.347301254450485, 2279.817638608977632 ) ) ;
#10337 = CIRCLE ( 'NONE', #9942, 0.7620000000000126672 ) ;
#10338 = APPROVAL_ROLE ( '' ) ;
#10339 = AXIS2_PLACEMENT_3D ( 'NONE', #4976, #17270, #15645 ) ;
#10340 = CARTESIAN_POINT ( 'NONE',  ( 110.6932000000009992, -3644.899999999999636, 2239.771999999999935 ) ) ;
#10341 = DIRECTION ( 'NONE',  ( 0.000000000000000000, 1.000000000000000000, 0.000000000000000000 ) ) ;
#10342 = CARTESIAN_POINT ( 'NONE',  ( 18.41147883874532099, -3579.724573821228660, 2244.678944975004924 ) ) ;
#10343 = TOROIDAL_SURFACE ( 'NONE', #18963, 5.588000000000000078, 0.7620000000000000107 ) ;
#10344 = CARTESIAN_POINT ( 'NONE',  ( 141.4924172101702595, -3657.295763141121370, 2247.322083679111529 ) ) ;
#10345 = CIRCLE ( 'NONE', #5501, 6.477000000000000313 ) ;
#10346 = VERTEX_POINT ( 'NONE', #23156 ) ;
#10347 = CARTESIAN_POINT ( 'NONE',  ( 15.03168679713838074, -3640.848700000155077, 2296.433984632765259 ) ) ;
#10348 = APPROVAL ( #23097, 'UNSPECIFIED' ) ;
#10349 = ORIENTED_EDGE ( 'NONE', *, *, #13960, .T. ) ;
#10350 = ORIENTED_EDGE ( 'NONE', *, *, #5216, .T. ) ;
#10351 = AXIS2_PLACEMENT_3D ( 'NONE', #4378, #18662, #2840 ) ;
#10352 = CARTESIAN_POINT ( 'NONE',  ( 15.24000000000000021, -3578.213872745999652, 2255.774000000000342 ) ) ;
#10353 = EDGE_CURVE ( 'NONE', #5628, #3849, #15566, .T. ) ;
#10354 = ORIENTED_EDGE ( 'NONE', *, *, #16396, .T. ) ;
#10355 = ORIENTED_EDGE ( 'NONE', *, *, #17971, .T. ) ;
#10356 = CARTESIAN_POINT ( 'NONE',  ( 151.1299999999999955, -3543.299999999999727, 2259.329999999999927 ) ) ;
#10357 = EDGE_CURVE ( 'NONE', #6867, #5052, #8462, .T. ) ;
#10358 = CARTESIAN_POINT ( 'NONE',  ( 12.69999999976724148, -3662.637340905157544, 2239.009999999999764 ) ) ;
#10359 = AXIS2_PLACEMENT_3D ( 'NONE', #21139, #12229, #17608 ) ;
#10360 = DIRECTION ( 'NONE',  ( -1.000000000000000000, 0.000000000000000000, 0.000000000000000000 ) ) ;
#10361 = EDGE_CURVE ( 'NONE', #18918, #10141, #15917, .T. ) ;
#10362 = ORIENTED_EDGE ( 'NONE', *, *, #5945, .F. ) ;
#10363 = CARTESIAN_POINT ( 'NONE',  ( 67.10679999999999268, -3644.899999999999636, 2260.600000000000364 ) ) ;
#10364 = CIRCLE ( 'NONE', #9256, 6.477000000001009283 ) ;
#10365 = DIRECTION ( 'NONE',  ( 0.000000000000000000, -1.000000000000000000, 0.000000000000000000 ) ) ;
#10366 = DIRECTION ( 'NONE',  ( 0.000000000000000000, -1.000000000000000000, 0.000000000000000000 ) ) ;
#10367 = LINE ( 'NONE', #12249, #5741 ) ;
#10368 = ORIENTED_EDGE ( 'NONE', *, *, #12385, .F. ) ;
#10369 = COORDINATED_UNIVERSAL_TIME_OFFSET ( 0, 0, .AHEAD. ) ;
#10370 = ORIENTED_EDGE ( 'NONE', *, *, #13639, .T. ) ;
#10371 = EDGE_CURVE ( 'NONE', #2446, #1205, #9947, .T. ) ;
#10372 = CARTESIAN_POINT ( 'NONE',  ( 9.987313202835000681, -3637.936329547143941, 2296.591799999999694 ) ) ;
#10373 = CARTESIAN_POINT ( 'NONE',  ( 10.06869043667276031, -3580.576266314660643, 2249.660797463413928 ) ) ;
#10374 = AXIS2_PLACEMENT_3D ( 'NONE', #16395, #10775, #21332 ) ;
#10375 = ADVANCED_FACE ( 'NONE', ( #8997 ), #21936, .T. ) ;
#10376 = ORIENTED_EDGE ( 'NONE', *, *, #5816, .F. ) ;
#10377 = FACE_BOUND ( 'NONE', #2382, .T. ) ;
#10378 = TOROIDAL_SURFACE ( 'NONE', #7764, 3.606799999999999784, 0.7620000000000000107 ) ;
#10379 = VECTOR ( 'NONE', #15477, 1000.000000000000114 ) ;
#10380 = VECTOR ( 'NONE', #4231, 1000.000000000000000 ) ;
#10381 = CARTESIAN_POINT ( 'NONE',  ( 12.69999999999999929, -3653.789999999999964, 2268.705139999999574 ) ) ;
#10382 = DIRECTION ( 'NONE',  ( -0.8660254037826616846, -0.5000000000030777603, 5.608020032299747518E-12 ) ) ;
#10383 = DIRECTION ( 'NONE',  ( -1.000000000000000000, 0.000000000000000000, 0.000000000000000000 ) ) ;
#10384 = CARTESIAN_POINT ( 'NONE',  ( 11.43159411791845059, -3662.051383365494985, 2249.499054103035633 ) ) ;
#10385 = CARTESIAN_POINT ( 'NONE',  ( 15.54478274857000031, -3659.509919104000346, 2250.166342301999521 ) ) ;
#10386 = ORIENTED_EDGE ( 'NONE', *, *, #14134, .F. ) ;
#10387 = DIRECTION ( 'NONE',  ( 0.000000000000000000, -1.000000000000000000, 0.000000000000000000 ) ) ;
#10388 = EDGE_CURVE ( 'NONE', #16359, #20183, #16150, .T. ) ;
#10389 = CARTESIAN_POINT ( 'NONE',  ( 12.69999999997316742, -3636.627870510297726, 2296.591799999996965 ) ) ;
#10390 = EDGE_CURVE ( 'NONE', #15239, #20703, #21560, .T. ) ;
#10391 = CIRCLE ( 'NONE', #4789, 2.844799999999994444 ) ;
#10392 = CARTESIAN_POINT ( 'NONE',  ( 136.8551999999999964, -3579.495007806000103, 2250.165025852999861 ) ) ;
#10393 = CARTESIAN_POINT ( 'NONE',  ( 15.20174512854452686, -3658.150442273887165, 2249.426080201244986 ) ) ;
#10394 = CYLINDRICAL_SURFACE ( 'NONE', #12071, 5.460999999999938126 ) ;
#10395 = ORIENTED_EDGE ( 'NONE', *, *, #7941, .F. ) ;
#10396 = VERTEX_POINT ( 'NONE', #1739 ) ;
#10397 = AXIS2_PLACEMENT_3D ( 'NONE', #2851, #13630, #20777 ) ;
#10398 = DIRECTION ( 'NONE',  ( -1.000000000000000000, 0.000000000000000000, 0.000000000000000000 ) ) ;
#10399 = ORIENTED_EDGE ( 'NONE', *, *, #12163, .T. ) ;
#10400 = CARTESIAN_POINT ( 'NONE',  ( 12.69997783158000004, -3636.657698770999559, 2279.817639764999967 ) ) ;
#10401 = DATE_TIME_ROLE ( 'classification_date' ) ;
#10402 = CARTESIAN_POINT ( 'NONE',  ( 20.32000000000000028, -3694.938000000000102, 2289.213099999999940 ) ) ;
#10403 = CARTESIAN_POINT ( 'NONE',  ( 11.36482343738000012, -3656.987758866999684, 2257.672197237000091 ) ) ;
#10404 = CARTESIAN_POINT ( 'NONE',  ( 66.34479999999999222, -3594.099999999999909, 2239.771999999999935 ) ) ;
#10405 = DIRECTION ( 'NONE',  ( 1.000000000000000000, 0.000000000000000000, 0.000000000000000000 ) ) ;
#10406 = CARTESIAN_POINT ( 'NONE',  ( 17.31138602735000021, -3576.119152860999748, 2246.630000000000109 ) ) ;
#10407 = AXIS2_PLACEMENT_3D ( 'NONE', #21824, #21709, #4015 ) ;
#10408 = CARTESIAN_POINT ( 'NONE',  ( 139.6999999999999886, -3659.504999999999654, 2272.030000000000200 ) ) ;
#10409 = ORIENTED_EDGE ( 'NONE', *, *, #18405, .T. ) ;
#10410 = CARTESIAN_POINT ( 'NONE',  ( 9.987313202740898177, -3581.061170452786428, 2239.009999999999764 ) ) ;
#10411 = CARTESIAN_POINT ( 'NONE',  ( -6.730999999999999872, -3578.860000000000127, 2247.392000000000280 ) ) ;
#10412 = VERTEX_POINT ( 'NONE', #8769 ) ;
#10413 = DIRECTION ( 'NONE',  ( -5.122214988120328377E-14, 0.000000000000000000, -1.000000000000000000 ) ) ;
#10414 = CARTESIAN_POINT ( 'NONE',  ( 10.29220312187077013, -3657.990044192180449, 2249.254950234671014 ) ) ;
#10415 = ORIENTED_EDGE ( 'NONE', *, *, #16303, .F. ) ;
#10416 = CARTESIAN_POINT ( 'NONE',  ( 6.984999999999000231, -3579.494999999999891, 2246.630000000000109 ) ) ;
#10417 = ORIENTED_EDGE ( 'NONE', *, *, #10811, .F. ) ;
#10418 = VERTEX_POINT ( 'NONE', #7026 ) ;
#10419 = EDGE_CURVE ( 'NONE', #16631, #17967, #11440, .T. ) ;
#10420 = DIRECTION ( 'NONE',  ( 0.000000000000000000, 0.000000000000000000, 1.000000000000000000 ) ) ;
#10421 = EDGE_CURVE ( 'NONE', #6713, #6778, #1336, .T. ) ;
#10422 = APPROVAL_ROLE ( '' ) ;
#10423 = ADVANCED_FACE ( 'NONE', ( #22887 ), #17623, .T. ) ;
#10424 = CARTESIAN_POINT ( 'NONE',  ( 15.54479999999932716, -3579.946214629475435, 2256.063560000000962 ) ) ;
#10425 = ORIENTED_EDGE ( 'NONE', *, *, #22294, .T. ) ;
#10426 = AXIS2_PLACEMENT_3D ( 'NONE', #22220, #2328, #7715 ) ;
#10427 = CARTESIAN_POINT ( 'NONE',  ( 132.0441057205090658, -3694.915156834097161, 2260.510101401284828 ) ) ;
#10428 = PERSON_AND_ORGANIZATION ( #5446, #1895 ) ;
#10429 = DIRECTION ( 'NONE',  ( -1.000000000000000000, -0.000000000000000000, -0.000000000000000000 ) ) ;
#10430 = CARTESIAN_POINT ( 'NONE',  ( 15.54479951278000094, -3579.494996001999880, 2250.165024905999871 ) ) ;
#10431 = EDGE_CURVE ( 'NONE', #18259, #8944, #3972, .T. ) ;
#10432 = FACE_BOUND ( 'NONE', #10445, .T. ) ;
#10433 = DIRECTION ( 'NONE',  ( 0.000000000000000000, -1.000000000000000000, 0.000000000000000000 ) ) ;
#10434 = FACE_OUTER_BOUND ( 'NONE', #13970, .T. ) ;
#10435 = ORIENTED_EDGE ( 'NONE', *, *, #7928, .F. ) ;
#10436 = DIRECTION ( 'NONE',  ( 0.000000000000000000, -1.000000000000000000, 0.000000000000000000 ) ) ;
#10437 = EDGE_CURVE ( 'NONE', #2616, #3620, #19318, .T. ) ;
#10438 = EDGE_CURVE ( 'NONE', #6304, #2568, #3212, .T. ) ;
#10439 = DIRECTION ( 'NONE',  ( 1.000000000000000000, 0.000000000000000000, 0.000000000000000000 ) ) ;
#10440 = VERTEX_POINT ( 'NONE', #15992 ) ;
#10441 = AXIS2_PLACEMENT_3D ( 'NONE', #19419, #3355, #17065 ) ;
#10442 = DIRECTION ( 'NONE',  ( 0.000000000000000000, 1.000000000000000000, 0.000000000000000000 ) ) ;
#10443 = CARTESIAN_POINT ( 'NONE',  ( 88.90000000000000568, -3644.899999999999636, 2239.771999999999935 ) ) ;
#10444 = VERTEX_POINT ( 'NONE', #10363 ) ;
#10445 = EDGE_LOOP ( 'NONE', ( #5986, #9039 ) ) ;
#10446 = VERTEX_POINT ( 'NONE', #8612 ) ;
#10447 = CARTESIAN_POINT ( 'NONE',  ( 1.270000000000000018, -3544.570000000000164, 2240.279999999999745 ) ) ;
#10448 = DIRECTION ( 'NONE',  ( 0.000000000000000000, -1.000000000000000000, 0.000000000000000000 ) ) ;
#10449 = ORIENTED_EDGE ( 'NONE', *, *, #11144, .T. ) ;
#10450 = CARTESIAN_POINT ( 'NONE',  ( 67.10679999999999268, -3644.899999999999636, 2239.009999999999764 ) ) ;
#10451 = EDGE_CURVE ( 'NONE', #8860, #18590, #6555, .T. ) ;
#10452 = DIRECTION ( 'NONE',  ( 0.000000000000000000, -0.5000000000006717960, 0.8660254037840506847 ) ) ;
#10453 = CARTESIAN_POINT ( 'NONE',  ( 12.69999999999999929, -3659.504999999999654, 2239.391000000000076 ) ) ;
#10454 = CARTESIAN_POINT ( 'NONE',  ( -0.7620000000000000107, -3544.061999999999898, 2253.487999999999829 ) ) ;
#10455 = CALENDAR_DATE ( 2026, 26, 10 ) ;
#10456 = AXIS2_PLACEMENT_3D ( 'NONE', #7217, #14367, #22783 ) ;
#10457 = LINE ( 'NONE', #15275, #5486 ) ;
#10458 = FACE_OUTER_BOUND ( 'NONE', #3993, .T. ) ;
#10459 = CARTESIAN_POINT ( 'NONE',  ( 18.37449373733476321, -3580.174051493370371, 2244.868862703829109 ) ) ;
#10460 = AXIS2_PLACEMENT_3D ( 'NONE', #15993, #19623, #3792 ) ;
#10461 = CARTESIAN_POINT ( 'NONE',  ( 142.1135160912012054, -3657.999060508418552, 2249.265414016712839 ) ) ;
#10462 = ORIENTED_EDGE ( 'NONE', *, *, #3269, .T. ) ;
#10463 = FACE_OUTER_BOUND ( 'NONE', #16514, .T. ) ;
#10464 = VERTEX_POINT ( 'NONE', #13886 ) ;
#10465 = ORIENTED_EDGE ( 'NONE', *, *, #13444, .T. ) ;
#10466 = ORIENTED_EDGE ( 'NONE', *, *, #15117, .T. ) ;
#10467 = DIRECTION ( 'NONE',  ( 0.000000000000000000, 0.000000000000000000, -1.000000000000000000 ) ) ;
#10468 = ORIENTED_EDGE ( 'NONE', *, *, #47, .T. ) ;
#10469 = VERTEX_POINT ( 'NONE', #6634 ) ;
#10470 = B_SPLINE_CURVE_WITH_KNOTS ( 'NONE', 3,
 ( #21639, #16581, #534, #7677 ),
 .UNSPECIFIED., .F., .F.,
 ( 4, 4 ),
 ( 0.9999968116805088014, 1.000000000000000000 ),
 .UNSPECIFIED. ) ;
#10471 = APPROVAL_PERSON_ORGANIZATION ( #4351, #1322, #21818 ) ;
#10472 = CARTESIAN_POINT ( 'NONE',  ( 4.909282597897117739, -3543.619369473608003, 2260.172357851842207 ) ) ;
#10473 = APPROVAL_STATUS ( 'not_yet_approved' ) ;
#10474 = DIRECTION ( 'NONE',  ( 0.000000000000000000, 0.000000000000000000, -1.000000000000000000 ) ) ;
#10475 = CARTESIAN_POINT ( 'NONE',  ( 101.5999999999999943, -3568.700000000000273, 2259.837999999999738 ) ) ;
#10476 = ORIENTED_EDGE ( 'NONE', *, *, #13590, .T. ) ;
#10477 = DIRECTION ( 'NONE',  ( 0.8660254037820785955, -0.5000000000040877302, -3.181634500919918361E-14 ) ) ;
#10478 = FACE_BOUND ( 'NONE', #14190, .T. ) ;
#10479 = FACE_OUTER_BOUND ( 'NONE', #9793, .T. ) ;
#10480 = FACE_OUTER_BOUND ( 'NONE', #6037, .T. ) ;
#10481 = EDGE_LOOP ( 'NONE', ( #10180, #6919, #19069, #19244 ) ) ;
#10482 = APPROVAL_DATE_TIME ( #13655, #1616 ) ;
#10483 = APPLIED_DATE_AND_TIME_ASSIGNMENT ( #9598, #18152, ( #28 ) ) ;
#10484 = VERTEX_POINT ( 'NONE', #19504 ) ;
#10485 = LINE ( 'NONE', #8508, #11286 ) ;
#10486 = B_SPLINE_CURVE_WITH_KNOTS ( 'NONE', 3,
 ( #4320, #16960, #10046, #6671, #5018, #4893, #20835, #17419, #4539, #9926, #22577, #1022, #17074, #2781, #20952, #22700 ),
 .UNSPECIFIED., .F., .F.,
 ( 4, 2, 2, 2, 2, 2, 2, 4 ),
 ( 2.950257753427574957E-08, 0.0005578634888370243754, 0.001115697475096514343, 0.001673531461356004418, 0.002231365447615494494, 0.003347033420134704930, 0.003904867406394249216, 0.004462701392653794369 ),
 .UNSPECIFIED. ) ;
#10487 = AXIS2_PLACEMENT_3D ( 'NONE', #2669, #11683, #9930 ) ;
#10488 = CARTESIAN_POINT ( 'NONE',  ( 10.44280607625477941, -3581.226489564329768, 2248.970834726309477 ) ) ;
#10489 = ADVANCED_FACE ( 'NONE', ( #12120 ), #7700, .T. ) ;
#10490 = CARTESIAN_POINT ( 'NONE',  ( 151.1299999999999955, -3578.860000000000127, 2251.506800000000112 ) ) ;
#10491 = CARTESIAN_POINT ( 'NONE',  ( 137.7873330486999919, -3657.399152860999493, 2246.630000000000109 ) ) ;
#10492 = APPROVAL_PERSON_ORGANIZATION ( #5805, #13489, #9316 ) ;
#10493 = EDGE_LOOP ( 'NONE', ( #9998, #5676, #17615, #3004 ) ) ;
#10494 = FACE_OUTER_BOUND ( 'NONE', #1782, .T. ) ;
#10495 = EDGE_CURVE ( 'NONE', #3918, #20823, #3583, .T. ) ;
#10496 = AXIS2_PLACEMENT_3D ( 'NONE', #9984, #4714, #11865 ) ;
#10497 = DIRECTION ( 'NONE',  ( 0.000000000000000000, 0.000000000000000000, -1.000000000000000000 ) ) ;
#10498 = CARTESIAN_POINT ( 'NONE',  ( 9.855200000000680305, -3579.946214629480892, 2256.063559999999597 ) ) ;
#10499 = DIRECTION ( 'NONE',  ( 0.000000000000000000, 1.000000000000000000, 0.000000000000000000 ) ) ;
#10500 = CARTESIAN_POINT ( 'NONE',  ( 12.44056639605545556, -3662.338708085364033, 2249.197182875595445 ) ) ;
#10501 = PRODUCT ( 'Screw 6', 'Screw 6', '', ( #13893 ) ) ;
#10502 = FACE_OUTER_BOUND ( 'NONE', #7080, .T. ) ;
#10503 = VERTEX_POINT ( 'NONE', #19275 ) ;
#10504 = DIRECTION ( 'NONE',  ( 1.000000000000000000, 0.000000000000000000, 0.000000000000000000 ) ) ;
#10505 = DIRECTION ( 'NONE',  ( 0.000000000000000000, -1.000000000000000000, 0.000000000000000000 ) ) ;
#10506 = LINE ( 'NONE', #16132, #23157 ) ;
#10507 = CARTESIAN_POINT ( 'NONE',  ( 14.81667057278108679, -3657.604317291794359, 2248.681661468295260 ) ) ;
#10508 = DIRECTION ( 'NONE',  ( -1.000000000000000000, 0.000000000000000000, 0.000000000000000000 ) ) ;
#10509 = APPLIED_SECURITY_CLASSIFICATION_ASSIGNMENT ( #20600, ( #23176 ) ) ;
#10510 = LOCAL_TIME ( 17, 37, 43.00000000000000000, #16113 ) ;
#10511 = DIRECTION ( 'NONE',  ( 0.000000000000000000, 0.000000000000000000, 1.000000000000000000 ) ) ;
#10512 = ORIENTED_EDGE ( 'NONE', *, *, #22697, .F. ) ;
#10513 = APPLIED_PERSON_AND_ORGANIZATION_ASSIGNMENT ( #17564, #3154, ( #22959 ) ) ;
#10514 = AXIS2_PLACEMENT_3D ( 'NONE', #16024, #12277, #87 ) ;
#10515 = DIRECTION ( 'NONE',  ( -2.318894227180156550E-14, -1.000000000000000000, 0.000000000000000000 ) ) ;
#10516 = CARTESIAN_POINT ( 'NONE',  ( 147.3199999999999932, -3694.430000000000291, 2260.600000000000364 ) ) ;
#10517 = ITEM_DEFINED_TRANSFORMATION ( 'NONE', 'NONE', #8624,  #5611 ) ;
#10518 = AXIS2_PLACEMENT_3D ( 'NONE', #2068, #21973, #312 ) ;
#10519 = DIRECTION ( 'NONE',  ( 1.000000000000000000, 0.000000000000000000, 0.000000000000000000 ) ) ;
#10520 = ADVANCED_FACE ( 'NONE', ( #5218 ), #6862, .T. ) ;
#10521 = CARTESIAN_POINT ( 'NONE',  ( 139.6999999999999886, -3584.956000000000131, 2244.978999999999814 ) ) ;
#10522 = FACE_OUTER_BOUND ( 'NONE', #12100, .T. ) ;
#10523 = EDGE_CURVE ( 'NONE', #12211, #15816, #17051, .T. ) ;
#10524 = LINE ( 'NONE', #20019, #7038 ) ;
#10525 = ADVANCED_FACE ( 'NONE', ( #21154 ), #18936, .T. ) ;
#10526 = PLANE ( 'NONE',  #3128 ) ;
#10527 = CARTESIAN_POINT ( 'NONE',  ( 12.69999999999999929, -3590.289999999999964, 2268.705139999999574 ) ) ;
#10528 = ORIENTED_EDGE ( 'NONE', *, *, #21537, .F. ) ;
#10529 =( BOUNDED_CURVE ( )  B_SPLINE_CURVE ( 3, ( #7489, #21446, #12765, #1632 ),
 .UNSPECIFIED., .F., .T. ) 
 B_SPLINE_CURVE_WITH_KNOTS ( ( 4, 4 ),
 ( 3.141592653589793116, 4.712388980444761621 ),
 .UNSPECIFIED. ) 
 CURVE ( )  GEOMETRIC_REPRESENTATION_ITEM ( )  RATIONAL_B_SPLINE_CURVE ( ( 1.000000000000000000, 0.8047378541102059302, 0.8047378541102059302, 1.000000000000000000 ) ) 
 REPRESENTATION_ITEM ( '' )  );
#10530 = CARTESIAN_POINT ( 'NONE',  ( -12.31900000000000084, -3660.140000000000327, 2247.392000000000280 ) ) ;
#10531 = LINE ( 'NONE', #19327, #14059 ) ;
#10532 = EDGE_LOOP ( 'NONE', ( #5516, #13641, #12984, #16440, #10055, #6504, #20509, #12871, #9659, #4429 ) ) ;
#10533 = LINE ( 'NONE', #12178, #22621 ) ;
#10534 = AXIS2_PLACEMENT_3D ( 'NONE', #16371, #2200, #7466 ) ;
#10535 = AXIS2_PLACEMENT_3D ( 'NONE', #21467, #10681, #19591 ) ;
#10536 = EDGE_LOOP ( 'NONE', ( #6606, #2262, #1387, #6581 ) ) ;
#10537 = CARTESIAN_POINT ( 'NONE',  ( 132.0583097651000060, -3694.797466901999996, 2260.545675974999995 ) ) ;
#10538 = EDGE_CURVE ( 'NONE', #22029, #16601, #21918, .T. ) ;
#10539 = B_SPLINE_CURVE_WITH_KNOTS ( 'NONE', 3,
 ( #15208, #479, #17299, #20062, #8409, #2898, #892, #9391, #15555, #20829, #1014, #5771, #10039, #15438, #2243, #22449, #11148 ),
 .UNSPECIFIED., .F., .F.,
 ( 4, 1, 1, 1, 1, 1, 1, 1, 1, 1, 1, 1, 1, 1, 4 ),
 ( 0.000000000000000000, 0.07142857142856999519, 0.1428571428570999946, 0.2142857142857000075, 0.2857142857143000203, 0.3571428571429000054, 0.4285714285713999594, 0.5000000000000000000, 0.5714285714286000406, 0.6428571428570999391, 0.7142857142856999797, 0.7857142857142999093, 0.8571428571429000609, 0.9285714285714000704, 1.000000000000000000 ),
 .UNSPECIFIED. ) ;
#10540 = ORIENTED_EDGE ( 'NONE', *, *, #10986, .F. ) ;
#10541 = ORIENTED_EDGE ( 'NONE', *, *, #9438, .F. ) ;
#10542 = CARTESIAN_POINT ( 'NONE',  ( 12.69999999999999929, -3589.528000000000247, 2268.705139999999574 ) ) ;
#10543 = SECURITY_CLASSIFICATION_LEVEL ( 'unclassified' ) ;
#10544 = CYLINDRICAL_SURFACE ( 'NONE', #10989, 0.7620000000000000107 ) ;
#10545 = VERTEX_POINT ( 'NONE', #10127 ) ;
#10546 = CARTESIAN_POINT ( 'NONE',  ( 12.69999999999999929, -3668.712499999999636, 2268.705139999999574 ) ) ;
#10547 = DATE_AND_TIME ( #15709, #14622 ) ;
#10548 = DIRECTION ( 'NONE',  ( -1.224646799147353207E-16, 1.000000000000000000, 0.000000000000000000 ) ) ;
#10549 = DIRECTION ( 'NONE',  ( 0.000000000000000000, 0.000000000000000000, -1.000000000000000000 ) ) ;
#10550 = AXIS2_PLACEMENT_3D ( 'NONE', #9318, #2282, #13165 ) ;
#10551 = DIRECTION ( 'NONE',  ( 0.000000000000000000, 1.000000000000000000, 0.000000000000000000 ) ) ;
#10552 = ADVANCED_FACE ( 'NONE', ( #3213 ), #17506, .T. ) ;
#10553 = DIRECTION ( 'NONE',  ( -1.000000000000000000, 0.000000000000000000, 0.000000000000000000 ) ) ;
#10554 = AXIS2_PLACEMENT_3D ( 'NONE', #5744, #12877, #9016 ) ;
#10555 = CARTESIAN_POINT ( 'NONE',  ( 1.270000000000000018, -3694.430000000000291, 2240.279999999999745 ) ) ;
#10556 = ORIENTED_EDGE ( 'NONE', *, *, #18733, .T. ) ;
#10557 = EDGE_CURVE ( 'NONE', #16518, #12839, #5117, .T. ) ;
#10558 = EDGE_CURVE ( 'NONE', #18858, #20500, #8378, .T. ) ;
#10559 = DIRECTION ( 'NONE',  ( 1.000000000000000000, 0.000000000000000000, 0.000000000000000000 ) ) ;
#10560 = ORIENTED_EDGE ( 'NONE', *, *, #503, .T. ) ;
#10561 = CARTESIAN_POINT ( 'NONE',  ( 4.836876043304535244, -3695.517456590399433, 2259.991366405333338 ) ) ;
#10562 = DIRECTION ( 'NONE',  ( -1.000000000000000000, 2.318894227180000040E-14, 2.343004830739999973E-14 ) ) ;
#10563 = AXIS2_PLACEMENT_3D ( 'NONE', #3920, #18216, #11068 ) ;
#10564 = DIRECTION ( 'NONE',  ( -1.000000000000000000, 0.000000000000000000, 0.000000000000000000 ) ) ;
#10565 = EDGE_LOOP ( 'NONE', ( #16781, #18235, #8786, #808 ) ) ;
#10566 = AXIS2_PLACEMENT_3D ( 'NONE', #21330, #3041, #19452 ) ;
#10567 = DIRECTION ( 'NONE',  ( 0.000000000000000000, 0.000000000000000000, -1.000000000000000000 ) ) ;
#10568 = ADVANCED_FACE ( 'NONE', ( #20916 ), #12005, .T. ) ;
#10569 = B_SPLINE_CURVE_WITH_KNOTS ( 'NONE', 3,
 ( #9172, #273, #7415, #605, #4120, #14912 ),
 .UNSPECIFIED., .F., .F.,
 ( 4, 1, 1, 4 ),
 ( 0.000000000000000000, 0.3333333333333000081, 0.6666666666667000474, 1.000000000000000000 ),
 .UNSPECIFIED. ) ;
#10570 = AXIS2_PLACEMENT_3D ( 'NONE', #8767, #15915, #23046 ) ;
#10571 = VERTEX_POINT ( 'NONE', #12596 ) ;
#10572 = AXIS2_PLACEMENT_3D ( 'NONE', #20363, #22114, #14980 ) ;
#10573 = DIRECTION ( 'NONE',  ( 0.000000000000000000, -1.000000000000000000, 0.000000000000000000 ) ) ;
#10574 = DIRECTION ( 'NONE',  ( 1.000000000000000000, 0.000000000000000000, 0.000000000000000000 ) ) ;
#10575 = SHAPE_REPRESENTATION_RELATIONSHIP ( 'NONE' , 'NONE' ,  #15665, #416 ) ;
#10576 = CARTESIAN_POINT ( 'NONE',  ( -6.731000000000127770, -3584.320999999999913, 2247.392000000000280 ) ) ;
#10577 = EDGE_CURVE ( 'NONE', #6733, #20297, #3912, .T. ) ;
#10578 = COORDINATED_UNIVERSAL_TIME_OFFSET ( 0, 0, .AHEAD. ) ;
#10579 = CARTESIAN_POINT ( 'NONE',  ( 88.90000000000000568, -3594.099999999999909, 2239.009999999999764 ) ) ;
#10580 = FACE_OUTER_BOUND ( 'NONE', #12764, .T. ) ;
#10581 = DIRECTION ( 'NONE',  ( -1.000000000000000000, 0.000000000000000000, -2.902585187577999742E-13 ) ) ;
#10582 = CIRCLE ( 'NONE', #18796, 2.844800000000091700 ) ;
#10583 = CARTESIAN_POINT ( 'NONE',  ( 137.2953324879588592, -3657.985077304744209, 2249.249213757072994 ) ) ;
#10584 = ORIENTED_EDGE ( 'NONE', *, *, #20279, .T. ) ;
#10585 = CARTESIAN_POINT ( 'NONE',  ( 0.000000000000000000, -3660.140000000000327, 2251.506800000000112 ) ) ;
#10586 = CIRCLE ( 'NONE', #3843, 2.844799999999994444 ) ;
#10587 = EDGE_CURVE ( 'NONE', #19668, #257, #3989, .T. ) ;
#10588 = ORIENTED_EDGE ( 'NONE', *, *, #9842, .T. ) ;
#10589 = ORIENTED_EDGE ( 'NONE', *, *, #4385, .F. ) ;
#10590 = EDGE_LOOP ( 'NONE', ( #16178, #22693 ) ) ;
#10591 = ORIENTED_EDGE ( 'NONE', *, *, #21943, .T. ) ;
#10592 = ORIENTED_EDGE ( 'NONE', *, *, #9365, .F. ) ;
#10593 = CARTESIAN_POINT ( 'NONE',  ( 4.837068669901056772, -3543.482543409432310, 2259.991289493689692 ) ) ;
#10594 = SECURITY_CLASSIFICATION_LEVEL ( 'unclassified' ) ;
#10595 = LINE ( 'NONE', #10122, #11391 ) ;
#10596 = AXIS2_PLACEMENT_3D ( 'NONE', #10290, #17198, #13458 ) ;
#10597 = DIRECTION ( 'NONE',  ( -0.8660254037839826280, -0.5000000000007898127, 0.000000000000000000 ) ) ;
#10598 = ORIENTED_EDGE ( 'NONE', *, *, #5401, .F. ) ;
#10599 = CARTESIAN_POINT ( 'NONE',  ( 12.69999999999999929, -3585.971999999999753, 2268.705139999999574 ) ) ;
#10600 = FACE_BOUND ( 'NONE', #4805, .T. ) ;
#10601 = DIRECTION ( 'NONE',  ( -1.000000000000000000, 0.000000000000000000, 0.000000000000000000 ) ) ;
#10602 = AXIS2_PLACEMENT_3D ( 'NONE', #4145, #13394, #18660 ) ;
#10603 = DIRECTION ( 'NONE',  ( 0.000000000000000000, 0.000000000000000000, -1.000000000000000000 ) ) ;
#10604 = ORIENTED_EDGE ( 'NONE', *, *, #9456, .F. ) ;
#10605 = EDGE_CURVE ( 'NONE', #2058, #14578, #22302, .T. ) ;
#10606 = APPLICATION_PROTOCOL_DEFINITION ( 'international standard', 'automotive_design', 2000, #483 ) ;
#10607 = AXIS2_PLACEMENT_3D ( 'NONE', #14552, #23084, #5646 ) ;
#10608 = CARTESIAN_POINT ( 'NONE',  ( 131.6470296322740126, -3543.300000000000182, 2259.515609114269409 ) ) ;
#10609 = CARTESIAN_POINT ( 'NONE',  ( 1.270000000000000018, -3544.570000000000164, 2260.600000000000364 ) ) ;
#10610 = EDGE_LOOP ( 'NONE', ( #13109, #21749, #9614 ) ) ;
#10611 = TOROIDAL_SURFACE ( 'NONE', #16972, 3.606799999999999784, 0.7620000000000000107 ) ;
#10612 = CARTESIAN_POINT ( 'NONE',  ( 19.17699999999999960, -3639.502500000000055, 2296.591799999999694 ) ) ;
#10613 = DIRECTION ( 'NONE',  ( 0.000000000000000000, 0.000000000000000000, -1.000000000000000000 ) ) ;
#10614 = DIRECTION ( 'NONE',  ( 1.000000000000000000, 0.000000000000000000, 0.000000000000000000 ) ) ;
#10615 = DIRECTION ( 'NONE',  ( 0.000000000000000000, 0.000000000000000000, 1.000000000000000000 ) ) ;
#10616 = CARTESIAN_POINT ( 'NONE',  ( 12.24081607761725543, -3662.313325058456030, 2249.227689240982272 ) ) ;
#10617 = APPROVAL ( #17192, 'UNKNOWN' ) ;
#10618 = CIRCLE ( 'NONE', #11727, 1.269999999999882334 ) ;
#10619 = CARTESIAN_POINT ( 'NONE',  ( 147.3321248976842242, -3544.290797603724968, 2260.569570596524045 ) ) ;
#10620 = VERTEX_POINT ( 'NONE', #20092 ) ;
#10621 = CARTESIAN_POINT ( 'NONE',  ( 124.1552000000010025, -3619.500000000000000, 2239.771999999999935 ) ) ;
#10622 = DIRECTION ( 'NONE',  ( 1.000000000000000000, 0.000000000000000000, 3.996303350731721563E-14 ) ) ;
#10623 = DIRECTION ( 'NONE',  ( 0.000000000000000000, 0.000000000000000000, -1.000000000000000000 ) ) ;
#10624 = CARTESIAN_POINT ( 'NONE',  ( 15.12638225371395073, -3658.019721843387288, 2249.289087668344564 ) ) ;
#10625 = CARTESIAN_POINT ( 'NONE',  ( 136.8684216348929965, -3695.579670241058011, 2255.043798072796562 ) ) ;
#10626 = AXIS2_PLACEMENT_3D ( 'NONE', #16853, #7965, #8773 ) ;
#10627 = ORIENTED_EDGE ( 'NONE', *, *, #17095, .F. ) ;
#10628 = CARTESIAN_POINT ( 'NONE',  ( 139.6999999999999886, -3657.599999999999909, 2272.030000000000200 ) ) ;
#10629 = CARTESIAN_POINT ( 'NONE',  ( 145.4149999194000316, -3579.495498070999474, 2244.618783703000190 ) ) ;
#10630 = APPROVAL_STATUS ( 'not_yet_approved' ) ;
#10631 = CARTESIAN_POINT ( 'NONE',  ( 12.69999999999999929, -3648.710000000000036, 2268.705139999999574 ) ) ;
#10632 = CARTESIAN_POINT ( 'NONE',  ( 9.903987878842999137, -3658.956623412000226, 2257.950097015999745 ) ) ;
#10633 = CARTESIAN_POINT ( 'NONE',  ( 137.1599999999999966, -3658.223872745999870, 2255.774000000000342 ) ) ;
#10634 = PLANE ( 'NONE',  #14492 ) ;
#10635 = DIRECTION ( 'NONE',  ( 0.5000000000047859494, 0.8660254037816754735, 0.000000000000000000 ) ) ;
#10636 = ORIENTED_EDGE ( 'NONE', *, *, #9797, .T. ) ;
#10637 = CARTESIAN_POINT ( 'NONE',  ( -12.69999999999999929, -3578.860000000000127, 2247.392000000000280 ) ) ;
#10638 = VERTEX_POINT ( 'NONE', #12474 ) ;
#10639 = VECTOR ( 'NONE', #11078, 1000.000000000000000 ) ;
#10640 = DIRECTION ( 'NONE',  ( 1.000000000000000000, 0.000000000000000000, 0.000000000000000000 ) ) ;
#10641 = PRODUCT_RELATED_PRODUCT_CATEGORY ( 'detail', '', ( #21176 ) ) ;
#10642 = TOROIDAL_SURFACE ( 'NONE', #17003, 3.606799999999999784, 0.7620000000000000107 ) ;
#10643 = CYLINDRICAL_SURFACE ( 'NONE', #3566, 2.844800000000091700 ) ;
#10644 = TOROIDAL_SURFACE ( 'NONE', #21494, 3.606799999999999784, 0.7620000000000000107 ) ;
#10645 = EDGE_LOOP ( 'NONE', ( #1829, #21920, #11881, #2041 ) ) ;
#10646 = CARTESIAN_POINT ( 'NONE',  ( 133.9849999999989905, -3579.494999999999891, 2246.630000000000109 ) ) ;
#10647 = EDGE_CURVE ( 'NONE', #6290, #2806, #4358, .T. ) ;
#10648 = ORIENTED_EDGE ( 'NONE', *, *, #9394, .F. ) ;
#10649 = DIRECTION ( 'NONE',  ( 1.000000000000000000, 0.000000000000000000, 0.000000000000000000 ) ) ;
#10650 = CARTESIAN_POINT ( 'NONE',  ( 12.69999999999999929, -3583.940000000000055, 2268.705139999999574 ) ) ;
#10651 = EDGE_CURVE ( 'NONE', #20183, #8499, #19974, .T. ) ;
#10652 = ORIENTED_EDGE ( 'NONE', *, *, #12219, .F. ) ;
#10653 = EDGE_CURVE ( 'NONE', #17044, #17328, #3561, .T. ) ;
#10654 = CARTESIAN_POINT ( 'NONE',  ( 136.9179185536690113, -3580.095427802566064, 2249.956228076800926 ) ) ;
#10655 = AXIS2_PLACEMENT_3D ( 'NONE', #16211, #21612, #17966 ) ;
#10656 = ORIENTED_EDGE ( 'NONE', *, *, #20537, .F. ) ;
#10657 = CARTESIAN_POINT ( 'NONE',  ( 54.40679999999999694, -3568.700000000000273, 2259.837999999999738 ) ) ;
#10658 = VECTOR ( 'NONE', #21965, 1000.000000000000000 ) ;
#10659 = APPROVAL_ROLE ( '' ) ;
#10660 = TOROIDAL_SURFACE ( 'NONE', #13656, 1.905000000000000027, 1.270000000000000018 ) ;
#10661 = AXIS2_PLACEMENT_3D ( 'NONE', #14235, #2164, #8840 ) ;
#10662 = CYLINDRICAL_SURFACE ( 'NONE', #8230, 2.844800000000091700 ) ;
#10663 = ADVANCED_FACE ( 'NONE', ( #2276 ), #19745, .F. ) ;
#10664 = CARTESIAN_POINT ( 'NONE',  ( 61.26424768829000556, -3544.061999999999898, 2279.827800000000025 ) ) ;
#10665 = CARTESIAN_POINT ( 'NONE',  ( 139.6999999999999886, -3579.494999999999891, 2245.359999999999673 ) ) ;
#10666 = CARTESIAN_POINT ( 'NONE',  ( 53.64479999999999649, -3568.700000000000273, 2239.771999999999935 ) ) ;
#10667 = EDGE_CURVE ( 'NONE', #17851, #12867, #7363, .T. ) ;
#10668 = DIRECTION ( 'NONE',  ( 0.000000000000000000, -1.000000000000000000, 0.000000000000000000 ) ) ;
#10669 = ORIENTED_EDGE ( 'NONE', *, *, #11943, .F. ) ;
#10670 = DIRECTION ( 'NONE',  ( 0.000000000000000000, 1.000000000000000000, 0.000000000000000000 ) ) ;
#10671 = CYLINDRICAL_SURFACE ( 'NONE', #21883, 0.3809999999999180154 ) ;
#10672 = ORIENTED_EDGE ( 'NONE', *, *, #341, .T. ) ;
#10673 = AXIS2_PLACEMENT_3D ( 'NONE', #15956, #10793, #20251 ) ;
#10674 = CARTESIAN_POINT ( 'NONE',  ( 3.175000000260485677, -3695.384369265535042, 2275.001800000000003 ) ) ;
#10675 = DIRECTION ( 'NONE',  ( -0.000000000000000000, 1.000000000000000000, 0.000000000000000000 ) ) ;
#10676 = AXIS2_PLACEMENT_3D ( 'NONE', #17611, #1617, #5030 ) ;
#10677 = AXIS2_PLACEMENT_3D ( 'NONE', #11223, #2323, #3847 ) ;
#10678 = PLANE ( 'NONE',  #4697 ) ;
#10679 = CIRCLE ( 'NONE', #16285, 2.844799999998995244 ) ;
#10680 = ORIENTED_EDGE ( 'NONE', *, *, #5698, .T. ) ;
#10681 = DIRECTION ( 'NONE',  ( 0.000000000000000000, -1.000000000000000000, 0.000000000000000000 ) ) ;
#10682 = DIRECTION ( 'NONE',  ( 1.000000000000000000, 0.000000000000000000, 0.000000000000000000 ) ) ;
#10683 = VERTEX_POINT ( 'NONE', #16339 ) ;
#10684 = EDGE_CURVE ( 'NONE', #1451, #13496, #10716, .T. ) ;
#10685 = DIRECTION ( 'NONE',  ( 1.000000000000000000, 0.000000000000000000, 0.000000000000000000 ) ) ;
#10686 = CARTESIAN_POINT ( 'NONE',  ( 139.6999999999999886, -3579.494999999999891, 2255.774000000000342 ) ) ;
#10687 = CARTESIAN_POINT ( 'NONE',  ( 17.62395365165161110, -3576.592063800514097, 2245.667268896361293 ) ) ;
#10688 = DIRECTION ( 'NONE',  ( -1.000000000000000000, -0.000000000000000000, -0.000000000000000000 ) ) ;
#10689 = PRODUCT_CONTEXT ( 'NONE', #3350, 'mechanical' ) ;
#10690 = EDGE_CURVE ( 'NONE', #2348, #9417, #3791, .T. ) ;
#10691 = CARTESIAN_POINT ( 'NONE',  ( 139.6999999999999886, -3659.504999999999654, 2239.391000000000076 ) ) ;
#10692 = CARTESIAN_POINT ( 'NONE',  ( 15.74707948048999917, -3695.699999999999818, 2254.503999999999905 ) ) ;
#10693 = EDGE_LOOP ( 'NONE', ( #20635, #4431, #3623, #10808 ) ) ;
#10694 = CARTESIAN_POINT ( 'NONE',  ( 1.270000000000000018, -3694.430000000000291, 2240.279999999999745 ) ) ;
#10695 = CIRCLE ( 'NONE', #21557, 2.844800000000091700 ) ;
#10696 = VECTOR ( 'NONE', #7005, 1000.000000000000000 ) ;
#10697 = PRODUCT_DEFINITION_SHAPE ( 'NONE', 'NONE',  #22796 ) ;
#10698 = CARTESIAN_POINT ( 'NONE',  ( 137.6640554538430194, -3657.517572872781784, 2248.495983249934852 ) ) ;
#10699 = VECTOR ( 'NONE', #12288, 1000.000000000000000 ) ;
#10700 = VECTOR ( 'NONE', #5029, 1000.000000000000000 ) ;
#10701 = ORIENTED_EDGE ( 'NONE', *, *, #21630, .T. ) ;
#10702 = CARTESIAN_POINT ( 'NONE',  ( 79.04479999999999507, -3670.300000000000182, 2261.869999999999891 ) ) ;
#10703 = ORIENTED_EDGE ( 'NONE', *, *, #16948, .T. ) ;
#10704 = ORIENTED_EDGE ( 'NONE', *, *, #13438, .T. ) ;
#10705 = ORIENTED_EDGE ( 'NONE', *, *, #11975, .F. ) ;
#10706 = CARTESIAN_POINT ( 'NONE',  ( 29.00679999999900005, -3670.300000000000182, 2259.837999999999738 ) ) ;
#10707 = ORIENTED_EDGE ( 'NONE', *, *, #13866, .F. ) ;
#10708 = EDGE_LOOP ( 'NONE', ( #14919, #4794, #223, #14321 ) ) ;
#10709 = CARTESIAN_POINT ( 'NONE',  ( 4.934152272631532554, -3543.678681369459810, 2260.234757311799058 ) ) ;
#10710 = AXIS2_PLACEMENT_3D ( 'NONE', #5327, #14123, #12472 ) ;
#10711 = COORDINATED_UNIVERSAL_TIME_OFFSET ( 0, 0, .AHEAD. ) ;
#10712 = DIRECTION ( 'NONE',  ( -2.848935406719999894E-12, 1.000000000000000000, 2.336881798978000141E-14 ) ) ;
#10713 = AXIS2_PLACEMENT_3D ( 'NONE', #10235, #8722, #4966 ) ;
#10714 = DIRECTION ( 'NONE',  ( 0.000000000000000000, 0.000000000000000000, -1.000000000000000000 ) ) ;
#10715 = ORIENTED_EDGE ( 'NONE', *, *, #22546, .T. ) ;
#10716 = CIRCLE ( 'NONE', #11106, 5.460999999999938126 ) ;
#10717 = CARTESIAN_POINT ( 'NONE',  ( -12.31900000000000084, -3657.790744320999693, 2248.748343399000532 ) ) ;
#10718 = FACE_BOUND ( 'NONE', #8803, .T. ) ;
#10719 = LINE ( 'NONE', #5451, #13219 ) ;
#10720 = LINE ( 'NONE', #21731, #18976 ) ;
#10721 = AXIS2_PLACEMENT_3D ( 'NONE', #18935, #22558, #13788 ) ;
#10722 = PERSON_AND_ORGANIZATION_ROLE ( 'creator' ) ;
#10723 = EDGE_CURVE ( 'NONE', #14933, #1252, #2167, .T. ) ;
#10724 = AXIS2_PLACEMENT_3D ( 'NONE', #11909, #10262, #15198 ) ;
#10725 = CARTESIAN_POINT ( 'NONE',  ( 131.8858812533569278, -3543.570688672563847, 2260.113808066775164 ) ) ;
#10726 = ADVANCED_FACE ( 'NONE', ( #18320 ), #9424, .T. ) ;
#10727 = CARTESIAN_POINT ( 'NONE',  ( -12.31900000000002393, -3661.486200000138069, 2245.060313203176065 ) ) ;
#10728 = DIRECTION ( 'NONE',  ( 1.000000000000000000, 0.000000000000000000, 0.000000000000000000 ) ) ;
#10729 = B_SPLINE_CURVE_WITH_KNOTS ( 'NONE', 3,
 ( #1429, #13856, #19248, #20892 ),
 .UNSPECIFIED., .F., .F.,
 ( 4, 4 ),
 ( 0.000000000000000000, 1.000000000000000000 ),
 .UNSPECIFIED. ) ;
#10730 = EDGE_LOOP ( 'NONE', ( #12566, #11853, #17024 ) ) ;
#10731 = CARTESIAN_POINT ( 'NONE',  ( 0.000000000000000000, -3695.699999999999818, 2260.600000000000364 ) ) ;
#10732 = AXIS2_PLACEMENT_3D ( 'NONE', #9753, #9987, #22515 ) ;
#10733 = DIRECTION ( 'NONE',  ( 1.319970543219000025E-14, -1.000000000000000000, -1.319970543219000025E-14 ) ) ;
#10734 = CARTESIAN_POINT ( 'NONE',  ( 10.16000000000000014, -3580.776127254000130, 2255.774000000000342 ) ) ;
#10735 = CIRCLE ( 'NONE', #6261, 0.7619999999999294005 ) ;
#10736 = CYLINDRICAL_SURFACE ( 'NONE', #21971, 6.349999999999855760 ) ;
#10737 = EDGE_CURVE ( 'NONE', #5364, #12671, #16445, .T. ) ;
#10738 = CARTESIAN_POINT ( 'NONE',  ( 50.79999999999999716, -3568.700000000000273, 2261.869999999999891 ) ) ;
#10739 = ADVANCED_FACE ( 'NONE', ( #398 ), #14699, .T. ) ;
#10740 = CARTESIAN_POINT ( 'NONE',  ( 9.855199999999999960, -3579.494999999999891, 2272.030000000000200 ) ) ;
#10741 = AXIS2_PLACEMENT_3D ( 'NONE', #21173, #14373, #5701 ) ;
#10742 = VERTEX_POINT ( 'NONE', #7091 ) ;
#10743 = FACE_OUTER_BOUND ( 'NONE', #812, .T. ) ;
#10744 = DIRECTION ( 'NONE',  ( 0.000000000000000000, 0.000000000000000000, -1.000000000000000000 ) ) ;
#10745 = CARTESIAN_POINT ( 'NONE',  ( 142.5208746554666561, -3579.068962104421644, 2250.236800009843137 ) ) ;
#10746 = CARTESIAN_POINT ( 'NONE',  ( 14.55205406967190029, -3657.345427267659488, 2247.931104812607373 ) ) ;
#10747 = CARTESIAN_POINT ( 'NONE',  ( -12.31900000000000084, -3577.513800000000174, 2249.723686796999573 ) ) ;
#10748 = VERTEX_POINT ( 'NONE', #21843 ) ;
#10749 = AXIS2_PLACEMENT_3D ( 'NONE', #12542, #18155, #17921 ) ;
#10750 = CARTESIAN_POINT ( 'NONE',  ( 110.6932000000009992, -3594.099999999999909, 2259.837999999999738 ) ) ;
#10751 = ORIENTED_EDGE ( 'NONE', *, *, #5665, .T. ) ;
#10752 = CIRCLE ( 'NONE', #4024, 3.606799999999993567 ) ;
#10753 = CARTESIAN_POINT ( 'NONE',  ( 22.54063073453000143, -3544.061999999999898, 2275.763800000000174 ) ) ;
#10754 = CARTESIAN_POINT ( 'NONE',  ( 10.16000000000000014, -3544.570000000000164, 2255.774000000000342 ) ) ;
#10755 = VECTOR ( 'NONE', #19434, 1000.000000000000000 ) ;
#10756 = CARTESIAN_POINT ( 'NONE',  ( 67.10679999999999268, -3594.099999999999909, 2239.009999999999764 ) ) ;
#10757 = AXIS2_PLACEMENT_3D ( 'NONE', #13953, #9963, #17111 ) ;
#10758 = DIRECTION ( 'NONE',  ( 0.000000000000000000, 0.000000000000000000, 1.000000000000000000 ) ) ;
#10759 = DIRECTION ( 'NONE',  ( 0.000000000000000000, 0.000000000000000000, -1.000000000000000000 ) ) ;
#10760 = CARTESIAN_POINT ( 'NONE',  ( 67.10679999999999268, -3594.099999999999909, 2259.837999999999738 ) ) ;
#10761 = ORIENTED_EDGE ( 'NONE', *, *, #16429, .T. ) ;
#10762 = CARTESIAN_POINT ( 'NONE',  ( 0.000000000000000000, -3544.061999999999898, 2295.829799999999977 ) ) ;
#10763 = ORIENTED_EDGE ( 'NONE', *, *, #21025, .F. ) ;
#10764 = DIRECTION ( 'NONE',  ( 0.000000000000000000, -1.000000000000000000, 0.000000000000000000 ) ) ;
#10765 = CIRCLE ( 'NONE', #14172, 2.844799999999994444 ) ;
#10766 = CARTESIAN_POINT ( 'NONE',  ( 20.32000000000000028, -3544.061999999999898, 2289.213099999999940 ) ) ;
#10767 = EDGE_LOOP ( 'NONE', ( #7592, #17682, #6967, #7430, #13847, #11340 ) ) ;
#10768 = DIRECTION ( 'NONE',  ( 0.000000000000000000, -1.000000000000000000, 0.000000000000000000 ) ) ;
#10769 = VERTEX_POINT ( 'NONE', #17864 ) ;
#10770 = CYLINDRICAL_SURFACE ( 'NONE', #8565, 2.844800000000091700 ) ;
#10771 = DIRECTION ( 'NONE',  ( -0.5000000000031962211, 0.8660254037825932949, 0.000000000000000000 ) ) ;
#10772 = ORIENTED_EDGE ( 'NONE', *, *, #9965, .T. ) ;
#10773 = CARTESIAN_POINT ( 'NONE',  ( 137.2840491909711602, -3580.996921585915516, 2249.269889241358214 ) ) ;
#10774 = EDGE_LOOP ( 'NONE', ( #22737, #17756, #19392, #13178 ) ) ;
#10775 = DIRECTION ( 'NONE',  ( 2.848812946084999742E-12, 1.000000000000000000, -2.336881798978000141E-14 ) ) ;
#10776 = DATE_TIME_ROLE ( 'classification_date' ) ;
#10777 = APPLIED_PERSON_AND_ORGANIZATION_ASSIGNMENT ( #13248, #16770, ( #11987 ) ) ;
#10778 = AXIS2_PLACEMENT_3D ( 'NONE', #8884, #23152, #7021 ) ;
#10779 = CARTESIAN_POINT ( 'NONE',  ( 101.5999999999999943, -3670.300000000000182, 2260.600000000000364 ) ) ;
#10780 = CARTESIAN_POINT ( 'NONE',  ( 12.69999999999999929, -3579.494999999999891, 2246.630000000000109 ) ) ;
#10781 = CARTESIAN_POINT ( 'NONE',  ( 76.20000000000000284, -3568.700000000000273, 2261.869999999999891 ) ) ;
#10782 = CARTESIAN_POINT ( 'NONE',  ( 127.0000000000000000, -3568.700000000000273, 2260.600000000000364 ) ) ;
#10783 = EDGE_CURVE ( 'NONE', #20178, #3840, #1810, .T. ) ;
#10784 = EDGE_CURVE ( 'NONE', #2750, #22532, #16220, .T. ) ;
#10785 = DIRECTION ( 'NONE',  ( -1.000000000000000000, 0.000000000000000000, 0.000000000000000000 ) ) ;
#10786 = ORIENTED_EDGE ( 'NONE', *, *, #12962, .F. ) ;
#10787 = CARTESIAN_POINT ( 'NONE',  ( 135.0886139726999886, -3576.119152860999748, 2246.630000000000109 ) ) ;
#10788 = EDGE_CURVE ( 'NONE', #22778, #19756, #13337, .T. ) ;
#10789 = CARTESIAN_POINT ( 'NONE',  ( 88.90000000000000568, -3594.099999999999909, 2259.837999999999738 ) ) ;
#10790 = ORIENTED_EDGE ( 'NONE', *, *, #5525, .F. ) ;
#10791 = CYLINDRICAL_SURFACE ( 'NONE', #15904, 5.715000000000999947 ) ;
#10792 = PLANE ( 'NONE',  #14744 ) ;
#10793 = DIRECTION ( 'NONE',  ( -2.336881798971000105E-14, 0.000000000000000000, -1.000000000000000000 ) ) ;
#10794 = ORIENTED_EDGE ( 'NONE', *, *, #21710, .F. ) ;
#10795 = ADVANCED_FACE ( 'NONE', ( #13498, #20316 ), #4257, .T. ) ;
#10796 = CARTESIAN_POINT ( 'NONE',  ( 14.71507054554999883, -3661.519743953000216, 2257.776232814999730 ) ) ;
#10797 = DIRECTION ( 'NONE',  ( 0.000000000000000000, 0.000000000000000000, 1.000000000000000000 ) ) ;
#10798 = ORIENTED_EDGE ( 'NONE', *, *, #220, .T. ) ;
#10799 = CARTESIAN_POINT ( 'NONE',  ( 91.74479999999999791, -3644.899999999999636, 2239.771999999999935 ) ) ;
#10800 = CARTESIAN_POINT ( 'NONE',  ( 15.03168679716000078, -3658.158799999999701, 2242.820000000000164 ) ) ;
#10801 =( NAMED_UNIT ( * ) SI_UNIT ( $, .STERADIAN. ) SOLID_ANGLE_UNIT ( ) );
#10802 = CARTESIAN_POINT ( 'NONE',  ( 0.000000000000000000, -3695.699999999999818, 2239.009999999999764 ) ) ;
#10803 = FACE_OUTER_BOUND ( 'NONE', #4909, .T. ) ;
#10804 = PERSON_AND_ORGANIZATION ( #5446, #1895 ) ;
#10805 = ORIENTED_EDGE ( 'NONE', *, *, #1679, .F. ) ;
#10806 = CARTESIAN_POINT ( 'NONE',  ( 59.89320000000000022, -3644.899999999999636, 2239.009999999999764 ) ) ;
#10807 = CARTESIAN_POINT ( 'NONE',  ( 10.11266208017212165, -3695.066554905903558, 2255.655544454599294 ) ) ;
#10808 = ORIENTED_EDGE ( 'NONE', *, *, #20587, .F. ) ;
#10809 = CARTESIAN_POINT ( 'NONE',  ( 18.25358222945826014, -3580.844011449823029, 2245.352786177662892 ) ) ;
#10810 = CARTESIAN_POINT ( 'NONE',  ( 137.8353954721896173, -3657.356297066692150, 2247.981376225718122 ) ) ;
#10811 = EDGE_CURVE ( 'NONE', #424, #6944, #17071, .T. ) ;
#10812 = VERTEX_POINT ( 'NONE', #11510 ) ;
#10813 = ORIENTED_EDGE ( 'NONE', *, *, #18901, .F. ) ;
#10814 = AXIS2_PLACEMENT_3D ( 'NONE', #3787, #10714, #12703 ) ;
#10815 = EDGE_CURVE ( 'NONE', #11168, #8878, #5878, .T. ) ;
#10816 = CARTESIAN_POINT ( 'NONE',  ( 137.9361976825551039, -3661.737158740789255, 2249.746205788910174 ) ) ;
#10817 = EDGE_CURVE ( 'NONE', #9389, #4126, #20421, .T. ) ;
#10818 = ORIENTED_EDGE ( 'NONE', *, *, #14245, .T. ) ;
#10819 = EDGE_LOOP ( 'NONE', ( #10468, #10466, #18973, #5206 ) ) ;
#10820 = ORIENTED_EDGE ( 'NONE', *, *, #17147, .F. ) ;
#10821 = CARTESIAN_POINT ( 'NONE',  ( 95.25000000000000000, -3694.430000000000291, 2251.506800000000112 ) ) ;
#10822 = ORIENTED_EDGE ( 'NONE', *, *, #17795, .T. ) ;
#10823 = ORIENTED_EDGE ( 'NONE', *, *, #21246, .T. ) ;
#10824 = CARTESIAN_POINT ( 'NONE',  ( 25.39999999999999858, -3568.700000000000273, 2261.869999999999891 ) ) ;
#10825 = SECURITY_CLASSIFICATION_LEVEL ( 'unclassified' ) ;
#10826 = CARTESIAN_POINT ( 'NONE',  ( 97.99320000000000164, -3670.300000000000182, 2239.009999999999764 ) ) ;
#10827 = DIRECTION ( 'NONE',  ( 0.000000000000000000, 1.000000000000000000, 0.000000000000000000 ) ) ;
#10828 = CIRCLE ( 'NONE', #10456, 1.270000000000000018 ) ;
#10829 = ORIENTED_EDGE ( 'NONE', *, *, #18163, .T. ) ;
#10830 = CARTESIAN_POINT ( 'NONE',  ( 61.26424768829000556, -3694.938000000000102, 2279.065800000000309 ) ) ;
#10831 = FACE_OUTER_BOUND ( 'NONE', #18939, .T. ) ;
#10832 = DIRECTION ( 'NONE',  ( -1.744130311077015631E-12, -0.5000000000049040771, -0.8660254037816071948 ) ) ;
#10833 = EDGE_CURVE ( 'NONE', #2356, #3639, #11458, .T. ) ;
#10834 = AXIS2_PLACEMENT_3D ( 'NONE', #7233, #19648, #14380 ) ;
#10835 = CARTESIAN_POINT ( 'NONE',  ( 139.6999999999999886, -3662.679999999999836, 2270.760000000000218 ) ) ;
#10836 = PERSON_AND_ORGANIZATION ( #5446, #1895 ) ;
#10837 = DIRECTION ( 'NONE',  ( 0.000000000000000000, 0.000000000000000000, 1.000000000000000000 ) ) ;
#10838 = ORIENTED_EDGE ( 'NONE', *, *, #14005, .T. ) ;
#10839 = DIRECTION ( 'NONE',  ( -1.000000000000000000, 0.000000000000000000, 0.000000000000000000 ) ) ;
#10840 = CARTESIAN_POINT ( 'NONE',  ( 151.4000000000000057, -3694.938000000000102, 2280.589800000000196 ) ) ;
#10841 = ORIENTED_EDGE ( 'NONE', *, *, #3476, .T. ) ;
#10842 = CARTESIAN_POINT ( 'NONE',  ( 20.82707948048999924, -3695.699999999999818, 2259.329999999999927 ) ) ;
#10843 = APPROVAL_PERSON_ORGANIZATION ( #17839, #10348, #16079 ) ;
#10844 = CARTESIAN_POINT ( 'NONE',  ( 17.78000000000000114, -3639.502500000000055, 2290.622800000000097 ) ) ;
#10845 = CARTESIAN_POINT ( 'NONE',  ( 15.03168679717383860, -3580.841200000147182, 2239.167815367294679 ) ) ;
#10846 = AXIS2_PLACEMENT_3D ( 'NONE', #13648, #11762, #3095 ) ;
#10847 = CARTESIAN_POINT ( 'NONE',  ( 57.14999999999999858, -3694.430000000000291, 2243.277199999999993 ) ) ;
#10848 = LINE ( 'NONE', #21636, #18136 ) ;
#10849 = ADVANCED_FACE ( 'NONE', ( #15271 ), #22171, .T. ) ;
#10850 = EDGE_CURVE ( 'NONE', #15231, #572, #15465, .T. ) ;
#10851 = CARTESIAN_POINT ( 'NONE',  ( 147.6115320350049274, -3543.420329759043398, 2259.869779574393760 ) ) ;
#10852 = EDGE_LOOP ( 'NONE', ( #7328, #19958, #15072, #17321 ) ) ;
#10853 = CARTESIAN_POINT ( 'NONE',  ( 95.25000000000000000, -3670.300000000000182, 2247.392000000000280 ) ) ;
#10854 = CARTESIAN_POINT ( 'NONE',  ( 12.69999999999999929, -3659.504999999999654, 2272.030000000000200 ) ) ;
#10855 = DIRECTION ( 'NONE',  ( 0.000000000000000000, 0.000000000000000000, 1.000000000000000000 ) ) ;
#10856 = CARTESIAN_POINT ( 'NONE',  ( 79.04479999999999507, -3568.700000000000273, 2259.837999999999738 ) ) ;
#10857 = CARTESIAN_POINT ( 'NONE',  ( 142.5315783651326456, -3543.420329758838761, 2255.043798072576010 ) ) ;
#10858 = CARTESIAN_POINT ( 'NONE',  ( 35.56000000000000227, -3568.700000000000273, 2247.392000000000280 ) ) ;
#10859 = ADVANCED_FACE ( 'NONE', ( #11355 ), #12220, .T. ) ;
#10860 = CARTESIAN_POINT ( 'NONE',  ( 7.776600320769382790, -3576.592737331526223, 2245.673273531844188 ) ) ;
#10861 = EDGE_LOOP ( 'NONE', ( #5035, #19437, #14106, #15078 ) ) ;
#10862 = VECTOR ( 'NONE', #19659, 1000.000000000000000 ) ;
#10863 = CARTESIAN_POINT ( 'NONE',  ( 0.7620000000000000107, -3544.061999999999898, 2239.009999999999764 ) ) ;
#10864 = PRODUCT_DEFINITION_FORMATION_WITH_SPECIFIED_SOURCE ( 'ANY', '', #16881, .NOT_KNOWN. ) ;
#10865 = DIRECTION ( 'NONE',  ( 0.000000000000000000, -1.000000000000000000, 0.000000000000000000 ) ) ;
#10866 = ADVANCED_FACE ( 'NONE', ( #2677 ), #22239, .T. ) ;
#10867 = LINE ( 'NONE', #21654, #12062 ) ;
#10868 = ADVANCED_FACE ( 'NONE', ( #9715 ), #18206, .T. ) ;
#10869 = DIRECTION ( 'NONE',  ( 0.000000000000000000, -1.000000000000000000, 0.000000000000000000 ) ) ;
#10870 = AXIS2_PLACEMENT_3D ( 'NONE', #5652, #14670, #7290 ) ;
#10871 = DIRECTION ( 'NONE',  ( 0.000000000000000000, 1.000000000000000000, 0.000000000000000000 ) ) ;
#10872 =( BOUNDED_CURVE ( )  B_SPLINE_CURVE ( 3, ( #5468, #3926, #7107, #14255 ),
 .UNSPECIFIED., .F., .T. ) 
 B_SPLINE_CURVE_WITH_KNOTS ( ( 4, 4 ),
 ( -2.664535259100375697E-14, 1.570796326449830138 ),
 .UNSPECIFIED. ) 
 CURVE ( )  GEOMETRIC_REPRESENTATION_ITEM ( )  RATIONAL_B_SPLINE_CURVE ( ( 1.000000000000000000, 0.8047378542056915496, 0.8047378542056915496, 1.000000000000000000 ) ) 
 REPRESENTATION_ITEM ( '' )  );
#10873 = DIRECTION ( 'NONE',  ( 0.000000000000000000, 0.000000000000000000, 1.000000000000000000 ) ) ;
#10874 = VERTEX_POINT ( 'NONE', #22473 ) ;
#10875 = FACE_OUTER_BOUND ( 'NONE', #12559, .T. ) ;
#10876 = ORIENTED_EDGE ( 'NONE', *, *, #20889, .T. ) ;
#10877 = AXIS2_PLACEMENT_3D ( 'NONE', #4297, #16378, #21655 ) ;
#10878 = CARTESIAN_POINT ( 'NONE',  ( 116.8400000000000034, -3670.300000000000182, 2247.392000000000280 ) ) ;
#10879 = EDGE_CURVE ( 'NONE', #2826, #15463, #14473, .T. ) ;
#10880 = CARTESIAN_POINT ( 'NONE',  ( 10.12686798322000215, -3638.275251157999719, 2279.515935650000301 ) ) ;
#10881 = VERTEX_POINT ( 'NONE', #2916 ) ;
#10882 = APPROVAL_PERSON_ORGANIZATION ( #16373, #18213, #9232 ) ;
#10883 = CARTESIAN_POINT ( 'NONE',  ( -6.349999999999880629, -3660.140000000000327, 2252.472000000000207 ) ) ;
#10884 = LOCAL_TIME ( 17, 37, 43.00000000000000000, #1402 ) ;
#10885 = ORIENTED_EDGE ( 'NONE', *, *, #13682, .F. ) ;
#10886 = CARTESIAN_POINT ( 'NONE',  ( 35.56000000000000227, -3670.300000000000182, 2247.392000000000280 ) ) ;
#10887 = CARTESIAN_POINT ( 'NONE',  ( 12.69999999999999929, -3659.504999999999654, 2272.030000000000200 ) ) ;
#10888 = VERTEX_POINT ( 'NONE', #10056 ) ;
#10889 = CARTESIAN_POINT ( 'NONE',  ( 137.7858121020460942, -3581.599504553262250, 2248.159153896805492 ) ) ;
#10890 = EDGE_LOOP ( 'NONE', ( #20588, #6211, #9002, #18831 ) ) ;
#10891 = FACE_OUTER_BOUND ( 'NONE', #22651, .T. ) ;
#10892 = APPROVAL_DATE_TIME ( #7266, #17344 ) ;
#10893 = EDGE_CURVE ( 'NONE', #9582, #15597, #15213, .T. ) ;
#10894 = LINE ( 'NONE', #245, #11958 ) ;
#10895 = VERTEX_POINT ( 'NONE', #11397 ) ;
#10896 = FACE_OUTER_BOUND ( 'NONE', #19048, .T. ) ;
#10897 = APPROVAL_PERSON_ORGANIZATION ( #10949, #15222, #21732 ) ;
#10898 = DIRECTION ( 'NONE',  ( 0.000000000000000000, 0.000000000000000000, -1.000000000000000000 ) ) ;
#10899 = DIRECTION ( 'NONE',  ( 2.336881798971000105E-14, 2.336881798971000105E-14, 1.000000000000000000 ) ) ;
#10900 = CARTESIAN_POINT ( 'NONE',  ( 139.2273618935608681, -3576.688940672205717, 2249.230374461885276 ) ) ;
#10901 = VERTEX_POINT ( 'NONE', #1032 ) ;
#10902 = CIRCLE ( 'NONE', #22860, 3.606799999998994366 ) ;
#10903 = CARTESIAN_POINT ( 'NONE',  ( 134.2331161326757751, -3577.829566977919512, 2244.740127772773121 ) ) ;
#10904 = CIRCLE ( 'NONE', #14660, 2.844799999998998796 ) ;
#10905 = CARTESIAN_POINT ( 'NONE',  ( 101.5999999999999943, -3568.700000000000273, 2259.837999999999738 ) ) ;
#10906 = ORIENTED_EDGE ( 'NONE', *, *, #910, .T. ) ;
#10908 = CARTESIAN_POINT ( 'NONE',  ( 11.36465921565999970, -3582.012152740000147, 2257.672217410000030 ) ) ;
#10907 = B_SPLINE_CURVE_WITH_KNOTS ( 'NONE', 3,
 ( #5588, #6595, #16690, #16574 ),
 .UNSPECIFIED., .F., .F.,
 ( 4, 4 ),
 ( 0.000000000000000000, 5.006989608022782729E-06 ),
 .UNSPECIFIED. ) ;
#10909 = CYLINDRICAL_SURFACE ( 'NONE', #10607, 2.844800000000091700 ) ;
#10910 = ORIENTED_EDGE ( 'NONE', *, *, #21106, .F. ) ;
#10911 = CARTESIAN_POINT ( 'NONE',  ( 14.50480255619999959, -3661.710066511000150, 2257.739429448999999 ) ) ;
#10912 = DIRECTION ( 'NONE',  ( 0.000000000000000000, -1.000000000000000000, 0.000000000000000000 ) ) ;
#10913 = ORIENTED_EDGE ( 'NONE', *, *, #22168, .T. ) ;
#10914 = FACE_OUTER_BOUND ( 'NONE', #20847, .T. ) ;
#10915 = CARTESIAN_POINT ( 'NONE',  ( 9.866830068855998448, -3639.817301451999811, 2279.450423099000091 ) ) ;
#10916 = CARTESIAN_POINT ( 'NONE',  ( 116.8400000000000034, -3568.700000000000273, 2244.547199999999975 ) ) ;
#10918 = DIRECTION ( 'NONE',  ( -1.000000000000000000, 0.000000000000000000, 2.324635735433000053E-14 ) ) ;
#10917 = AXIS2_PLACEMENT_3D ( 'NONE', #1901, #12222, #5196 ) ;
#10919 = APPROVAL_ROLE ( '' ) ;
#10920 = ORIENTED_EDGE ( 'NONE', *, *, #20232, .F. ) ;
#10921 = TOROIDAL_SURFACE ( 'NONE', #13918, 3.606799999999999784, 0.7620000000000000107 ) ;
#10922 = CARTESIAN_POINT ( 'NONE',  ( -12.31900000000000084, -3578.860000000000127, 2247.392000000000280 ) ) ;
#10923 = DIRECTION ( 'NONE',  ( -5.122214988120328377E-14, 0.000000000000000000, -1.000000000000000000 ) ) ;
#10924 = ORIENTED_EDGE ( 'NONE', *, *, #16148, .T. ) ;
#10925 = LINE ( 'NONE', #12570, #2140 ) ;
#10926 = CARTESIAN_POINT ( 'NONE',  ( 137.4644108502616291, -3657.744905272460983, 2248.928881783665020 ) ) ;
#10927 = EDGE_LOOP ( 'NONE', ( #9698, #7770 ) ) ;
#10928 = AXIS2_PLACEMENT_3D ( 'NONE', #2052, #7444, #406 ) ;
#10929 = CARTESIAN_POINT ( 'NONE',  ( 140.8259220789218205, -3662.117874465443492, 2249.436863160725807 ) ) ;
#10930 = VERTEX_POINT ( 'NONE', #20604 ) ;
#10931 = VERTEX_POINT ( 'NONE', #1148 ) ;
#10932 = AXIS2_PLACEMENT_3D ( 'NONE', #22040, #15447, #6005 ) ;
#10933 = PRODUCT_DEFINITION ( 'UNKNOWN', '', #13121, #9477 ) ;
#10934 = CIRCLE ( 'NONE', #13190, 2.844799999999994444 ) ;
#10935 = CARTESIAN_POINT ( 'NONE',  ( 12.69999999999999929, -3639.502500000000055, 2295.829799999999977 ) ) ;
#10936 = ORIENTED_EDGE ( 'NONE', *, *, #1932, .T. ) ;
#10937 = EDGE_LOOP ( 'NONE', ( #3619, #11383, #4799 ) ) ;
#10938 = CARTESIAN_POINT ( 'NONE',  ( 117.9067999999989951, -3644.899999999999636, 2259.837999999999738 ) ) ;
#10939 = CARTESIAN_POINT ( 'NONE',  ( 64.76999999999999602, -3695.699999999999818, 2285.606299999999919 ) ) ;
#10940 = CARTESIAN_POINT ( 'NONE',  ( 10.16000000000000014, -3660.786127253999894, 2255.774000000000342 ) ) ;
#10941 = ORIENTED_EDGE ( 'NONE', *, *, #7926, .T. ) ;
#10942 = CARTESIAN_POINT ( 'NONE',  ( -12.31900000000000084, -3578.860000000000127, 2247.392000000000280 ) ) ;
#10943 = EDGE_CURVE ( 'NONE', #14640, #7743, #8863, .T. ) ;
#10944 = DIRECTION ( 'NONE',  ( 0.000000000000000000, 0.000000000000000000, 1.000000000000000000 ) ) ;
#10945 = DIRECTION ( 'NONE',  ( 0.000000000000000000, 0.000000000000000000, 1.000000000000000000 ) ) ;
#10946 = EDGE_CURVE ( 'NONE', #12925, #15061, #7850, .T. ) ;
#10947 = CARTESIAN_POINT ( 'NONE',  ( 57.14999999999999858, -3670.300000000000182, 2247.392000000000280 ) ) ;
#10948 = CIRCLE ( 'NONE', #831, 0.7619999999999987894 ) ;
#10949 = PERSON_AND_ORGANIZATION ( #5446, #1895 ) ;
#10950 = EDGE_CURVE ( 'NONE', #22478, #5090, #14839, .T. ) ;
#10951 = ORIENTED_EDGE ( 'NONE', *, *, #1403, .T. ) ;
#10952 = CARTESIAN_POINT ( 'NONE',  ( 139.6999999999999886, -3668.712499999999636, 2257.592639999999847 ) ) ;
#10953 = ORIENTED_EDGE ( 'NONE', *, *, #14605, .F. ) ;
#10954 = AXIS2_PLACEMENT_3D ( 'NONE', #12359, #17272, #19159 ) ;
#10955 = AXIS2_PLACEMENT_3D ( 'NONE', #4651, #22692, #22917 ) ;
#10956 = DIRECTION ( 'NONE',  ( 1.000000000000000000, 0.000000000000000000, 8.741913579724000206E-14 ) ) ;
#10957 = CARTESIAN_POINT ( 'NONE',  ( 7.845716004698516599, -3662.521111503330303, 2245.835192429324707 ) ) ;
#10958 = VERTEX_POINT ( 'NONE', #6563 ) ;
#10959 = DIRECTION ( 'NONE',  ( 0.000000000000000000, -1.000000000000000000, 0.000000000000000000 ) ) ;
#10960 = EDGE_CURVE ( 'NONE', #11664, #20457, #16338, .T. ) ;
#10961 = CARTESIAN_POINT ( 'NONE',  ( 139.6999999999999886, -3579.494999999999891, 2272.030000000000200 ) ) ;
#10962 = FACE_OUTER_BOUND ( 'NONE', #12303, .T. ) ;
#10963 = AXIS2_PLACEMENT_3D ( 'NONE', #18876, #9966, #1059 ) ;
#10964 = DIRECTION ( 'NONE',  ( 0.000000000000000000, -1.000000000000000000, 0.000000000000000000 ) ) ;
#10965 = ORIENTED_EDGE ( 'NONE', *, *, #17064, .T. ) ;
#10966 = CARTESIAN_POINT ( 'NONE',  ( 18.01287425285000410, -3657.399152860999493, 2246.630000000000109 ) ) ;
#10967 = ORIENTED_EDGE ( 'NONE', *, *, #15657, .F. ) ;
#10968 = CARTESIAN_POINT ( 'NONE',  ( 147.3359700947606825, -3694.748620250581098, 2260.560053407111354 ) ) ;
#10969 = DIRECTION ( 'NONE',  ( -0.8660254037820102058, 0.5000000000042060799, 1.814359422182020449E-12 ) ) ;
#10970 = AXIS2_PLACEMENT_3D ( 'NONE', #10453, #13857, #6720 ) ;
#10971 = DIRECTION ( 'NONE',  ( 0.000000000000000000, 1.000000000000000000, 0.000000000000000000 ) ) ;
#10972 = VECTOR ( 'NONE', #6834, 1000.000000000000000 ) ;
#10973 = CARTESIAN_POINT ( 'NONE',  ( -6.730999999999999872, -3578.860000000000127, 2247.392000000000280 ) ) ;
#10974 = FACE_OUTER_BOUND ( 'NONE', #2892, .T. ) ;
#10975 = CARTESIAN_POINT ( 'NONE',  ( 136.8581157282275740, -3695.591362401052720, 2255.017974340396904 ) ) ;
#10976 = CARTESIAN_POINT ( 'NONE',  ( 7.166763845495746743, -3578.065052041517447, 2244.660461834260786 ) ) ;
#10977 = ORIENTED_EDGE ( 'NONE', *, *, #2664, .F. ) ;
#10978 = CALENDAR_DATE ( 2026, 26, 10 ) ;
#10979 = EDGE_CURVE ( 'NONE', #9004, #4452, #699, .T. ) ;
#10980 = CYLINDRICAL_SURFACE ( 'NONE', #10534, 2.844800000000091700 ) ;
#10981 = DIRECTION ( 'NONE',  ( 0.000000000000000000, 0.000000000000000000, 1.000000000000000000 ) ) ;
#10983 = CIRCLE ( 'NONE', #857, 2.844799999999994444 ) ;
#10982 = DATE_AND_TIME ( #21653, #20999 ) ;
#10984 = EDGE_CURVE ( 'NONE', #18142, #12726, #979, .T. ) ;
#10985 = FACE_OUTER_BOUND ( 'NONE', #22538, .T. ) ;
#10986 = EDGE_CURVE ( 'NONE', #5628, #2574, #19705, .T. ) ;
#10987 = CIRCLE ( 'NONE', #13980, 3.175000000000149925 ) ;
#10988 = LINE ( 'NONE', #4066, #4492 ) ;
#10989 = AXIS2_PLACEMENT_3D ( 'NONE', #8450, #14066, #15706 ) ;
#10990 = DIRECTION ( 'NONE',  ( 1.000000000000000000, 0.000000000000000000, 0.000000000000000000 ) ) ;
#10991 = VECTOR ( 'NONE', #10206, 1000.000000000000000 ) ;
#10992 = DIRECTION ( 'NONE',  ( 0.000000000000000000, 0.000000000000000000, 1.000000000000000000 ) ) ;
#10993 = ORIENTED_EDGE ( 'NONE', *, *, #12448, .T. ) ;
#10994 = DIRECTION ( 'NONE',  ( -1.000000000000000000, 0.000000000000000000, 0.000000000000000000 ) ) ;
#10995 = CARTESIAN_POINT ( 'NONE',  ( 11.76748838596000013, -3636.808600170000318, 2279.779819357000179 ) ) ;
#10996 = ORIENTED_EDGE ( 'NONE', *, *, #11707, .T. ) ;
#10997 = CARTESIAN_POINT ( 'NONE',  ( 8.520528180907378513, -3657.399153627112355, 2246.629997243945581 ) ) ;
#10998 = CIRCLE ( 'NONE', #22573, 2.844799999999999773 ) ;
#10999 = EDGE_CURVE ( 'NONE', #5650, #1650, #15934, .T. ) ;
#11000 = EDGE_LOOP ( 'NONE', ( #8309, #8831, #1445, #13214, #8231 ) ) ;
#11001 = FACE_OUTER_BOUND ( 'NONE', #8920, .T. ) ;
#11002 = DIRECTION ( 'NONE',  ( 1.000000000000000000, 0.000000000000000000, 0.000000000000000000 ) ) ;
#11003 = ORIENTED_EDGE ( 'NONE', *, *, #3865, .T. ) ;
#11004 = CARTESIAN_POINT ( 'NONE',  ( 137.1708602166628737, -3580.797675544396043, 2249.475566895118391 ) ) ;
#11005 = ORIENTED_EDGE ( 'NONE', *, *, #9394, .T. ) ;
#11006 = CARTESIAN_POINT ( 'NONE',  ( 0.7620000000000000107, -3544.061999999999898, 2239.771999999999935 ) ) ;
#11007 =( BOUNDED_CURVE ( )  B_SPLINE_CURVE ( 3, ( #5971, #897, #9700, #14877 ),
 .UNSPECIFIED., .F., .T. ) 
 B_SPLINE_CURVE_WITH_KNOTS ( ( 4, 4 ),
 ( -9.769962616701377556E-15, 1.570796326937976328 ),
 .UNSPECIFIED. ) 
 CURVE ( )  GEOMETRIC_REPRESENTATION_ITEM ( )  RATIONAL_B_SPLINE_CURVE ( ( 1.000000000000000000, 0.8047378540906384714, 0.8047378540906384714, 1.000000000000000000 ) ) 
 REPRESENTATION_ITEM ( '' )  );
#11008 = APPROVAL_DATE_TIME ( #9261, #19805 ) ;
#11009 = ADVANCED_FACE ( 'NONE', ( #7967 ), #20495, .F. ) ;
#11010 = DIRECTION ( 'NONE',  ( 0.000000000000000000, 0.000000000000000000, -1.000000000000000000 ) ) ;
#11011 = CARTESIAN_POINT ( 'NONE',  ( 47.95519999999999783, -3670.300000000000182, 2239.771999999999935 ) ) ;
#11012 = AXIS2_PLACEMENT_3D ( 'NONE', #3142, #22709, #3026 ) ;
#11013 = CARTESIAN_POINT ( 'NONE',  ( -12.70000000000005436, -3581.992340905245783, 2247.392000000001644 ) ) ;
#11014 = DIRECTION ( 'NONE',  ( 0.000000000000000000, 0.000000000000000000, -1.000000000000000000 ) ) ;
#11015 = CARTESIAN_POINT ( 'NONE',  ( 142.2803686719938128, -3578.294778489228975, 2250.180949407634216 ) ) ;
#11016 = ORIENTED_EDGE ( 'NONE', *, *, #19546, .T. ) ;
#11017 = CARTESIAN_POINT ( 'NONE',  ( 134.8379986833869282, -3576.491331054022794, 2245.816465486069319 ) ) ;
#11018 = ORIENTED_EDGE ( 'NONE', *, *, #14722, .F. ) ;
#11019 = DIRECTION ( 'NONE',  ( -1.000000000000000000, 0.000000000000000000, 0.000000000000000000 ) ) ;
#11020 = ORIENTED_EDGE ( 'NONE', *, *, #4278, .F. ) ;
#11021 = DIRECTION ( 'NONE',  ( 0.000000000000000000, 0.000000000000000000, 1.000000000000000000 ) ) ;
#11022 = DIRECTION ( 'NONE',  ( 0.000000000000000000, 0.000000000000000000, -1.000000000000000000 ) ) ;
#11023 = EDGE_CURVE ( 'NONE', #15874, #18712, #21919, .T. ) ;
#11024 = EDGE_CURVE ( 'NONE', #2750, #19558, #18940, .T. ) ;
#11025 = EDGE_LOOP ( 'NONE', ( #645, #5783, #8923, #7554, #3201, #11914, #6826, #14668, #15462 ) ) ;
#11026 = DIRECTION ( 'NONE',  ( 0.000000000000000000, 0.000000000000000000, 1.000000000000000000 ) ) ;
#11027 = DIRECTION ( 'NONE',  ( 1.000000000000000000, 0.000000000000000000, 0.000000000000000000 ) ) ;
#11028 = AXIS2_PLACEMENT_3D ( 'NONE', #11327, #22327, #14968 ) ;
#11029 = VERTEX_POINT ( 'NONE', #8775 ) ;
#11030 = AXIS2_PLACEMENT_3D ( 'NONE', #17995, #14606, #1713 ) ;
#11031 = DIRECTION ( 'NONE',  ( 0.000000000000000000, 0.000000000000000000, 1.000000000000000000 ) ) ;
#11032 = CARTESIAN_POINT ( 'NONE',  ( -5.588000000000000078, -3578.860000000000127, 2247.392000000000280 ) ) ;
#11033 = CARTESIAN_POINT ( 'NONE',  ( 141.5863318965145652, -3581.624734270543740, 2246.715920429194739 ) ) ;
#11034 = ORIENTED_EDGE ( 'NONE', *, *, #2416, .F. ) ;
#11035 = CARTESIAN_POINT ( 'NONE',  ( 139.6999999999985675, -3662.379629489635590, 2239.010000000083437 ) ) ;
#11036 = PERSON_AND_ORGANIZATION ( #5446, #1895 ) ;
#11037 = VERTEX_POINT ( 'NONE', #19086 ) ;
#11038 = CYLINDRICAL_SURFACE ( 'NONE', #16377, 0.3810000000000011156 ) ;
#11039 = CARTESIAN_POINT ( 'NONE',  ( 116.8400000000000034, -3670.300000000000182, 2247.392000000000280 ) ) ;
#11040 = EDGE_LOOP ( 'NONE', ( #7429, #15139, #16606, #11322, #14364, #7800 ) ) ;
#11041 = LINE ( 'NONE', #16202, #14538 ) ;
#11042 = CARTESIAN_POINT ( 'NONE',  ( 137.5807515951455855, -3657.607188378255159, 2248.687286021772707 ) ) ;
#11043 = AXIS2_PLACEMENT_3D ( 'NONE', #10209, #19355, #1423 ) ;
#11044 = ORIENTED_EDGE ( 'NONE', *, *, #8454, .F. ) ;
#11045 = AXIS2_PLACEMENT_3D ( 'NONE', #20110, #5819, #12950 ) ;
#11046 = CARTESIAN_POINT ( 'NONE',  ( 138.2235839798819370, -3661.937167866388336, 2249.597460511887220 ) ) ;
#11047 = CIRCLE ( 'NONE', #6941, 1.270000000000000240 ) ;
#11048 = ORIENTED_EDGE ( 'NONE', *, *, #19172, .F. ) ;
#11049 = CIRCLE ( 'NONE', #17389, 0.7619999999999294005 ) ;
#11050 = EDGE_LOOP ( 'NONE', ( #16804, #16049, #13064, #6383 ) ) ;
#11051 = ORIENTED_EDGE ( 'NONE', *, *, #19383, .F. ) ;
#11052 = DIRECTION ( 'NONE',  ( 0.000000000000000000, 0.000000000000000000, -1.000000000000000000 ) ) ;
#11053 = EDGE_LOOP ( 'NONE', ( #1441, #9692, #11935, #12236, #18984 ) ) ;
#11054 = ORIENTED_EDGE ( 'NONE', *, *, #2834, .F. ) ;
#11055 = PLANE ( 'NONE',  #18756 ) ;
#11056 = ORIENTED_EDGE ( 'NONE', *, *, #5435, .T. ) ;
#11057 = DIRECTION ( 'NONE',  ( -1.000000000000000000, 0.000000000000000000, 0.000000000000000000 ) ) ;
#11058 = CARTESIAN_POINT ( 'NONE',  ( 12.69999999999999929, -3585.210000000000036, 2262.355140000000119 ) ) ;
#11059 = AXIS2_PLACEMENT_3D ( 'NONE', #5007, #21298, #5240 ) ;
#11060 = CIRCLE ( 'NONE', #10676, 1.269999999999882334 ) ;
#11061 = DIRECTION ( 'NONE',  ( 1.000000000000000000, 0.000000000000000000, 0.000000000000000000 ) ) ;
#11062 = DATE_TIME_ROLE ( 'creation_date' ) ;
#11063 = AXIS2_PLACEMENT_3D ( 'NONE', #20575, #5960, #2890 ) ;
#11064 = CARTESIAN_POINT ( 'NONE',  ( 132.0441057203201467, -3544.084843163416281, 2260.510101400297117 ) ) ;
#11065 = ORIENTED_EDGE ( 'NONE', *, *, #18440, .T. ) ;
#11066 = CIRCLE ( 'NONE', #14069, 3.606800000000021100 ) ;
#11067 = APPLIED_DATE_AND_TIME_ASSIGNMENT ( #2280, #11183, ( #22059 ) ) ;
#11068 = DIRECTION ( 'NONE',  ( 0.000000000000000000, 0.000000000000000000, 1.000000000000000000 ) ) ;
#11069 = EDGE_CURVE ( 'NONE', #5355, #12999, #4647, .T. ) ;
#11070 = DIRECTION ( 'NONE',  ( 1.122008997397786234E-13, 0.000000000000000000, -1.000000000000000000 ) ) ;
#11071 = AXIS2_PLACEMENT_3D ( 'NONE', #10340, #4830, #17486 ) ;
#11072 = DIRECTION ( 'NONE',  ( 0.000000000000000000, 0.000000000000000000, -1.000000000000000000 ) ) ;
#11073 = EDGE_LOOP ( 'NONE', ( #20209, #22902, #7885, #20709 ) ) ;
#11074 = FACE_OUTER_BOUND ( 'NONE', #8193, .T. ) ;
#11075 = ADVANCED_FACE ( 'NONE', ( #19208 ), #3263, .T. ) ;
#11076 = ADVANCED_FACE ( 'NONE', ( #10295 ), #8550, .F. ) ;
#11077 = AXIS2_PLACEMENT_3D ( 'NONE', #11640, #15409, #8259 ) ;
#11078 = DIRECTION ( 'NONE',  ( 0.000000000000000000, 0.000000000000000000, 1.000000000000000000 ) ) ;
#11079 = B_SPLINE_CURVE_WITH_KNOTS ( 'NONE', 3,
 ( #1544, #8702, #15496, #15848, #20894, #11978, #19131, #17245, #22979, #14095, #6609, #6485, #3069, #13622, #20768, #11866, #1188 ),
 .UNSPECIFIED., .F., .F.,
 ( 4, 1, 1, 1, 1, 1, 1, 1, 1, 1, 1, 1, 1, 1, 4 ),
 ( 0.000000000000000000, 0.07142857142856999519, 0.1428571428570999946, 0.2142857142857000075, 0.2857142857143000203, 0.3571428571429000054, 0.4285714285713999594, 0.5000000000000000000, 0.5714285714286000406, 0.6428571428570999391, 0.7142857142856999797, 0.7857142857142999093, 0.8571428571429000609, 0.9285714285714000704, 0.9999948892526789868 ),
 .UNSPECIFIED. ) ;
#11080 = CARTESIAN_POINT ( 'NONE',  ( 12.69999999999999929, -3659.504999999999654, 2245.359999999999673 ) ) ;
#11081 = VECTOR ( 'NONE', #9442, 1000.000000000000000 ) ;
#11082 = CYLINDRICAL_SURFACE ( 'NONE', #18883, 2.844800000000091700 ) ;
#11083 = PRODUCT_DEFINITION_SHAPE ( 'NONE', 'NONE',  #23167 ) ;
#11085 = ORIENTED_EDGE ( 'NONE', *, *, #1813, .T. ) ;
#11084 = ADVANCED_FACE ( 'NONE', ( #8431 ), #1498, .F. ) ;
#11086 = AXIS2_PLACEMENT_3D ( 'NONE', #19079, #1141, #19320 ) ;
#11087 = FACE_OUTER_BOUND ( 'NONE', #4496, .T. ) ;
#11088 = ORIENTED_EDGE ( 'NONE', *, *, #15136, .F. ) ;
#11089 = CARTESIAN_POINT ( 'NONE',  ( 147.4095600311624708, -3695.151712726811184, 2260.375808267130651 ) ) ;
#11090 = DIRECTION ( 'NONE',  ( -1.000000000000000000, 0.000000000000000000, 0.000000000000000000 ) ) ;
#11091 = VECTOR ( 'NONE', #14370, 1000.000000000000000 ) ;
#11092 = CARTESIAN_POINT ( 'NONE',  ( 12.69999999999999929, -3599.497499999999945, 2296.210799999999836 ) ) ;
#11093 = AXIS2_PLACEMENT_3D ( 'NONE', #6806, #15704, #8447 ) ;
#11094 = DIRECTION ( 'NONE',  ( -1.000000000000000000, 0.000000000000000000, 0.000000000000000000 ) ) ;
#11095 = CARTESIAN_POINT ( 'NONE',  ( 92.50679999999999836, -3644.899999999999636, 2260.600000000000364 ) ) ;
#11096 = EDGE_CURVE ( 'NONE', #6733, #13716, #8894, .T. ) ;
#11097 = DIRECTION ( 'NONE',  ( -1.000000000000000000, 0.000000000000000000, 0.000000000000000000 ) ) ;
#11098 = CARTESIAN_POINT ( 'NONE',  ( 7.483768054671388725, -3577.160018264615701, 2245.111000847615287 ) ) ;
#11099 = ORIENTED_EDGE ( 'NONE', *, *, #6677, .T. ) ;
#11100 = DATE_AND_TIME ( #3390, #21725 ) ;
#11101 = CARTESIAN_POINT ( 'NONE',  ( -12.69999999998383977, -3661.577314745246440, 2249.881502164247649 ) ) ;
#11102 = EDGE_CURVE ( 'NONE', #9663, #13850, #4906, .T. ) ;
#11103 = CARTESIAN_POINT ( 'NONE',  ( 95.25000000000000000, -3543.299999999999727, 2247.392000000000280 ) ) ;
#11104 = CONTEXT_DEPENDENT_SHAPE_REPRESENTATION ( #21771, #18754 ) ;
#11105 = DIRECTION ( 'NONE',  ( -1.224646799147353207E-16, 1.000000000000000000, 0.000000000000000000 ) ) ;
#11106 = AXIS2_PLACEMENT_3D ( 'NONE', #10942, #292, #11179 ) ;
#11107 = DIRECTION ( 'NONE',  ( 0.000000000000000000, 1.000000000000000000, 0.000000000000000000 ) ) ;
#11108 = VECTOR ( 'NONE', #15505, 1000.000000000000114 ) ;
#11109 = ORIENTED_EDGE ( 'NONE', *, *, #3835, .F. ) ;
#11110 = CARTESIAN_POINT ( 'NONE',  ( 142.5447999999989861, -3579.494999999999891, 2272.030000000000200 ) ) ;
#11111 = ORIENTED_EDGE ( 'NONE', *, *, #14831, .F. ) ;
#11112 = DIRECTION ( 'NONE',  ( 1.000000000000000000, 1.730170395987999916E-13, 0.000000000000000000 ) ) ;
#11113 = ORIENTED_EDGE ( 'NONE', *, *, #3814, .F. ) ;
#11114 = ADVANCED_FACE ( 'NONE', ( #15578, #14177, #6792 ), #21320, .F. ) ;
#11115 = DIRECTION ( 'NONE',  ( -1.000000000000000000, 0.000000000000000000, 0.000000000000000000 ) ) ;
#11116 = EDGE_CURVE ( 'NONE', #20980, #861, #22268, .T. ) ;
#11117 = LINE ( 'NONE', #20245, #2108 ) ;
#11118 = ORIENTED_EDGE ( 'NONE', *, *, #21642, .T. ) ;
#11119 = DIRECTION ( 'NONE',  ( 0.000000000000000000, 0.000000000000000000, 1.000000000000000000 ) ) ;
#11120 = CIRCLE ( 'NONE', #12291, 0.7619999999999987894 ) ;
#11121 = AXIS2_PLACEMENT_3D ( 'NONE', #4146, #1075, #18893 ) ;
#11122 = ORIENTED_EDGE ( 'NONE', *, *, #6454, .T. ) ;
#11123 = CARTESIAN_POINT ( 'NONE',  ( 142.2706172139890839, -3694.866442832754728, 2255.697297438070564 ) ) ;
#11124 = CARTESIAN_POINT ( 'NONE',  ( 151.4000000000000057, -3543.299999999999727, 2275.001800000000003 ) ) ;
#11125 = VERTEX_POINT ( 'NONE', #13934 ) ;
#11126 = CIRCLE ( 'NONE', #10741, 6.477000000000000313 ) ;
#11127 = CARTESIAN_POINT ( 'NONE',  ( 137.5670226385637704, -3581.377374464106197, 2248.717048606296885 ) ) ;
#11128 = EDGE_CURVE ( 'NONE', #5084, #5090, #16301, .T. ) ;
#11129 = ORIENTED_EDGE ( 'NONE', *, *, #22315, .T. ) ;
#11130 = CYLINDRICAL_SURFACE ( 'NONE', #3649, 2.844799999999999773 ) ;
#11131 = COORDINATED_UNIVERSAL_TIME_OFFSET ( 0, 0, .AHEAD. ) ;
#11132 = LINE ( 'NONE', #9372, #5983 ) ;
#11133 = DIRECTION ( 'NONE',  ( 1.000000000000000000, 0.000000000000000000, 0.000000000000000000 ) ) ;
#11134 = CARTESIAN_POINT ( 'NONE',  ( 64.76999999999999602, -3694.938000000000102, 2289.213099999999940 ) ) ;
#11135 = AXIS2_PLACEMENT_3D ( 'NONE', #2141, #21817, #5550 ) ;
#11136 = CARTESIAN_POINT ( 'NONE',  ( 140.2422887712748718, -3576.687509671706266, 2249.232688864233751 ) ) ;
#11137 = ORIENTED_EDGE ( 'NONE', *, *, #20942, .T. ) ;
#11138 = CARTESIAN_POINT ( 'NONE',  ( 134.1907311445957589, -3577.975272958113692, 2244.688205607437339 ) ) ;
#11139 = CIRCLE ( 'NONE', #19369, 0.7619999999999294005 ) ;
#11140 = DIRECTION ( 'NONE',  ( 1.000000000000000000, 0.000000000000000000, 0.000000000000000000 ) ) ;
#11141 = VERTEX_POINT ( 'NONE', #12175 ) ;
#11142 = DIRECTION ( 'NONE',  ( 0.000000000000000000, -1.000000000000000000, 0.000000000000000000 ) ) ;
#11143 = CARTESIAN_POINT ( 'NONE',  ( 15.55719817093123680, -3543.392327578681943, 2254.979458604820138 ) ) ;
#11144 = EDGE_CURVE ( 'NONE', #18508, #18837, #12939, .T. ) ;
#11145 = ORIENTED_EDGE ( 'NONE', *, *, #11782, .F. ) ;
#11146 = EDGE_CURVE ( 'NONE', #21667, #21114, #9929, .T. ) ;
#11147 = CARTESIAN_POINT ( 'NONE',  ( 151.1299999999999955, -3694.430000000000291, 2240.279999999999745 ) ) ;
#11148 = CARTESIAN_POINT ( 'NONE',  ( 12.69997932225824400, -3596.652698770999905, 2279.817639835496266 ) ) ;
#11149 = VERTEX_POINT ( 'NONE', #5260 ) ;
#11150 = VECTOR ( 'NONE', #8182, 1000.000000000000000 ) ;
#11151 = DIRECTION ( 'NONE',  ( -0.5000000000031962211, 0.8660254037825932949, 0.000000000000000000 ) ) ;
#11152 = CARTESIAN_POINT ( 'NONE',  ( 10.66697763051307035, -3577.504112144065402, 2249.893375748385552 ) ) ;
#11153 = DIRECTION ( 'NONE',  ( 1.000000000000000000, 0.000000000000000000, 0.000000000000000000 ) ) ;
#11154 = FACE_BOUND ( 'NONE', #13, .T. ) ;
#11155 = ADVANCED_FACE ( 'NONE', ( #12295 ), #7136, .T. ) ;
#11156 = ORIENTED_EDGE ( 'NONE', *, *, #10390, .T. ) ;
#11157 = CARTESIAN_POINT ( 'NONE',  ( 151.1299999999999955, -3694.430000000000291, 2239.009999999999764 ) ) ;
#11158 = PRODUCT_CONTEXT ( 'NONE', #16793, 'mechanical' ) ;
#11159 = AXIS2_PLACEMENT_3D ( 'NONE', #9657, #22291, #16795 ) ;
#11160 = DIRECTION ( 'NONE',  ( 0.000000000000000000, 1.000000000000000000, 0.000000000000000000 ) ) ;
#11161 = CARTESIAN_POINT ( 'NONE',  ( 0.000000000000000000, -3694.938000000000102, 2253.487999999999829 ) ) ;
#11162 = VERTEX_POINT ( 'NONE', #11936 ) ;
#11163 = CARTESIAN_POINT ( 'NONE',  ( -12.69999999986526795, -3661.577314745183230, 2244.902497835854774 ) ) ;
#11164 = ADVANCED_FACE ( 'NONE', ( #10174 ), #17319, .F. ) ;
#11165 = DIRECTION ( 'NONE',  ( -2.324635735433000053E-14, 0.000000000000000000, -1.000000000000000000 ) ) ;
#11166 = ADVANCED_FACE ( 'NONE', ( #20024 ), #14520, .F. ) ;
#11167 = ORIENTED_EDGE ( 'NONE', *, *, #21618, .T. ) ;
#11168 = VERTEX_POINT ( 'NONE', #14633 ) ;
#11169 = CARTESIAN_POINT ( 'NONE',  ( 140.3978084557461443, -3662.263276882629725, 2249.285383685099077 ) ) ;
#11170 = AXIS2_PLACEMENT_3D ( 'NONE', #14624, #849, #13399 ) ;
#11171 = VERTEX_POINT ( 'NONE', #2099 ) ;
#11172 = ORIENTED_EDGE ( 'NONE', *, *, #13804, .F. ) ;
#11173 = EDGE_CURVE ( 'NONE', #12078, #23061, #2210, .T. ) ;
#11174 = DIRECTION ( 'NONE',  ( 3.194481088216070180E-14, 0.5000000000047110094, 0.8660254037817188832 ) ) ;
#11175 = ORIENTED_EDGE ( 'NONE', *, *, #6869, .T. ) ;
#11176 = CARTESIAN_POINT ( 'NONE',  ( 12.69999999999999929, -3585.971999999999753, 2262.355140000000119 ) ) ;
#11177 = DIRECTION ( 'NONE',  ( 0.000000000000000000, -1.000000000000000000, 0.000000000000000000 ) ) ;
#11178 = EDGE_LOOP ( 'NONE', ( #19098, #19611, #22674, #11336 ) ) ;
#11179 = DIRECTION ( 'NONE',  ( -2.318894227180156550E-14, -1.000000000000000000, 0.000000000000000000 ) ) ;
#11180 = DIRECTION ( 'NONE',  ( -1.000000000000000000, -0.000000000000000000, -0.000000000000000000 ) ) ;
#11181 = CARTESIAN_POINT ( 'NONE',  ( 7.332978169984068373, -3581.459545042232548, 2246.234697006676925 ) ) ;
#11182 = CARTESIAN_POINT ( 'NONE',  ( 139.6999999999999886, -3659.504999999999654, 2244.978999999999814 ) ) ;
#11183 = DATE_TIME_ROLE ( 'classification_date' ) ;
#11184 = CARTESIAN_POINT ( 'NONE',  ( 139.6999999999999886, -3659.504999999999654, 2270.760000000000218 ) ) ;
#11185 = TOROIDAL_SURFACE ( 'NONE', #12674, 3.606799999999999784, 0.7620000000000000107 ) ;
#11186 = CARTESIAN_POINT ( 'NONE',  ( -5.588000000000000078, -3694.938000000000102, 2254.250000000000000 ) ) ;
#11187 = ORIENTED_EDGE ( 'NONE', *, *, #5868, .F. ) ;
#11188 = CARTESIAN_POINT ( 'NONE',  ( 7.052475312426777165, -3660.425490918647938, 2244.547175452708416 ) ) ;
#11189 = ORIENTED_EDGE ( 'NONE', *, *, #16997, .F. ) ;
#11190 = CARTESIAN_POINT ( 'NONE',  ( 10.16000000000000014, -3695.699999999999818, 2255.774000000000342 ) ) ;
#11191 = PLANE ( 'NONE',  #17381 ) ;
#11192 = FACE_OUTER_BOUND ( 'NONE', #17256, .T. ) ;
#11193 = CARTESIAN_POINT ( 'NONE',  ( -12.69999999985380867, -3581.734629489801137, 2247.392000000001644 ) ) ;
#11194 = ORIENTED_EDGE ( 'NONE', *, *, #9487, .F. ) ;
#11195 = CARTESIAN_POINT ( 'NONE',  ( 18.10176712835724189, -3657.638581454599716, 2246.036268407943226 ) ) ;
#11196 = EDGE_LOOP ( 'NONE', ( #10233, #3451, #6481, #19380 ) ) ;
#11197 = CARTESIAN_POINT ( 'NONE',  ( 147.4512129905548932, -3695.282573427842635, 2260.271345400768041 ) ) ;
#11198 = CARTESIAN_POINT ( 'NONE',  ( 141.0563433985999779, -3661.854255679000289, 2239.391000000000076 ) ) ;
#11199 = TOROIDAL_SURFACE ( 'NONE', #20934, 6.476999999999000224, 0.7620000000000000107 ) ;
#11200 = CARTESIAN_POINT ( 'NONE',  ( 15.03168679714000078, -3638.156300000000101, 2292.781800000000203 ) ) ;
#11201 = APPROVAL ( #17686, 'UNSPECIFIED' ) ;
#11202 = CARTESIAN_POINT ( 'NONE',  ( 15.03168679714000078, -3598.151299999999992, 2292.781800000000203 ) ) ;
#11203 = DIRECTION ( 'NONE',  ( 0.000000000000000000, 0.000000000000000000, 1.000000000000000000 ) ) ;
#11204 = PLANE ( 'NONE',  #20677 ) ;
#11205 = CARTESIAN_POINT ( 'NONE',  ( 7.733373459861585530, -3576.666886843865541, 2245.578275576291617 ) ) ;
#11206 = ORIENTED_EDGE ( 'NONE', *, *, #4101, .T. ) ;
#11207 = COORDINATED_UNIVERSAL_TIME_OFFSET ( 0, 0, .AHEAD. ) ;
#11208 = EDGE_CURVE ( 'NONE', #20939, #13646, #18554, .T. ) ;
#11209 = VERTEX_POINT ( 'NONE', #9127 ) ;
#11210 = CARTESIAN_POINT ( 'NONE',  ( 1.270000000000000018, -3544.570000000000164, 2259.329999999999927 ) ) ;
#11211 = AXIS2_PLACEMENT_3D ( 'NONE', #21166, #8743, #14137 ) ;
#11212 = EDGE_CURVE ( 'NONE', #1446, #16063, #3842, .T. ) ;
#11213 = CARTESIAN_POINT ( 'NONE',  ( 10.36831320283000046, -3640.848700000000008, 2292.781800000000203 ) ) ;
#11214 = DIRECTION ( 'NONE',  ( -1.000000000000000000, 0.000000000000000000, 0.000000000000000000 ) ) ;
#11215 = ORIENTED_EDGE ( 'NONE', *, *, #4541, .T. ) ;
#11216 = CARTESIAN_POINT ( 'NONE',  ( 114.2999999999999972, -3644.899999999999636, 2239.771999999999935 ) ) ;
#11217 = ORIENTED_EDGE ( 'NONE', *, *, #12705, .F. ) ;
#11218 = CARTESIAN_POINT ( 'NONE',  ( 35.56000000000000227, -3568.700000000000273, 2247.392000000000280 ) ) ;
#11219 = ORIENTED_EDGE ( 'NONE', *, *, #16954, .F. ) ;
#11220 = CYLINDRICAL_SURFACE ( 'NONE', #13301, 2.844799999998995244 ) ;
#11221 = LINE ( 'NONE', #20026, #12952 ) ;
#11222 = ORIENTED_EDGE ( 'NONE', *, *, #6935, .T. ) ;
#11223 = CARTESIAN_POINT ( 'NONE',  ( -8.890000000018000392, -3658.793800000000374, 2249.723686796999573 ) ) ;
#11224 = PLANE ( 'NONE',  #3564 ) ;
#11225 = CIRCLE ( 'NONE', #7849, 4.114799999999974034 ) ;
#11226 = PRODUCT_DEFINITION ( 'UNKNOWN', '', #20249, #570 ) ;
#11227 = VERTEX_POINT ( 'NONE', #331 ) ;
#11228 = CARTESIAN_POINT ( 'NONE',  ( 114.2999999999999972, -3594.099999999999909, 2259.837999999999738 ) ) ;
#11229 = CARTESIAN_POINT ( 'NONE',  ( 101.5999999999999943, -3619.500000000000000, 2259.837999999999738 ) ) ;
#11230 = PRODUCT_DEFINITION_FORMATION_WITH_SPECIFIED_SOURCE ( 'ANY', '', #19099, .NOT_KNOWN. ) ;
#11231 = ORIENTED_EDGE ( 'NONE', *, *, #18822, .F. ) ;
#11232 = EDGE_CURVE ( 'NONE', #3301, #4102, #9574, .T. ) ;
#11233 = DIRECTION ( 'NONE',  ( 0.000000000000000000, -1.000000000000000000, 0.000000000000000000 ) ) ;
#11234 = ORIENTED_EDGE ( 'NONE', *, *, #20515, .F. ) ;
#11235 = DIRECTION ( 'NONE',  ( 1.000000000000000000, 0.000000000000000000, 1.344294159210000097E-14 ) ) ;
#11236 = PERSON_AND_ORGANIZATION ( #5446, #1895 ) ;
#11237 = ADVANCED_FACE ( 'NONE', ( #18252 ), #8071, .T. ) ;
#11238 = LINE ( 'NONE', #12768, #1481 ) ;
#11239 = CARTESIAN_POINT ( 'NONE',  ( 18.24372733278048386, -3660.894223056912324, 2244.648543520397652 ) ) ;
#11240 = AXIS2_PLACEMENT_3D ( 'NONE', #17660, #5253, #17779 ) ;
#11241 = DIRECTION ( 'NONE',  ( -0.000000000000000000, -1.000000000000000000, -0.000000000000000000 ) ) ;
#11242 = CARTESIAN_POINT ( 'NONE',  ( 145.4032257520333360, -3659.928912255530122, 2244.547217120886671 ) ) ;
#11243 = SECURITY_CLASSIFICATION ( '', '', #14762 ) ;
#11244 = CARTESIAN_POINT ( 'NONE',  ( 141.4814987657295546, -3577.276937191656998, 2249.755702771833512 ) ) ;
#11245 = ORIENTED_EDGE ( 'NONE', *, *, #827, .F. ) ;
#11246 = APPROVAL_PERSON_ORGANIZATION ( #17334, #4186, #15132 ) ;
#11247 = EDGE_LOOP ( 'NONE', ( #4468, #12813 ) ) ;
#11248 = DIRECTION ( 'NONE',  ( -1.000000000000000000, 0.000000000000000000, 0.000000000000000000 ) ) ;
#11249 = AXIS2_PLACEMENT_3D ( 'NONE', #8232, #3068, #8701 ) ;
#11250 = ORIENTED_EDGE ( 'NONE', *, *, #22157, .T. ) ;
#11251 = EDGE_CURVE ( 'NONE', #15997, #9478, #12186, .T. ) ;
#11252 = CARTESIAN_POINT ( 'NONE',  ( 12.80540911176254859, -3596.652697124181941, 2279.817639555324604 ) ) ;
#11253 = CARTESIAN_POINT ( 'NONE',  ( 15.41071740316960614, -3543.619369471847676, 2255.346357850129607 ) ) ;
#11254 = ORIENTED_EDGE ( 'NONE', *, *, #5203, .T. ) ;
#11255 = DIRECTION ( 'NONE',  ( 0.000000000000000000, 0.000000000000000000, 1.000000000000000000 ) ) ;
#11256 = CARTESIAN_POINT ( 'NONE',  ( -12.69999999999997087, -3575.727659094874525, 2247.391999999782001 ) ) ;
#11257 = ORIENTED_EDGE ( 'NONE', *, *, #818, .F. ) ;
#11258 = CYLINDRICAL_SURFACE ( 'NONE', #1992, 2.844799999999994444 ) ;
#11259 = CARTESIAN_POINT ( 'NONE',  ( 12.00521842515822790, -3576.735947014849899, 2249.284512218476721 ) ) ;
#11260 = APPROVAL_PERSON_ORGANIZATION ( #8647, #6767, #5369 ) ;
#11261 = CARTESIAN_POINT ( 'NONE',  ( 12.70000000023333264, -3602.629840905158289, 2296.591799999999694 ) ) ;
#11262 = ORIENTED_EDGE ( 'NONE', *, *, #15017, .T. ) ;
#11263 = APPROVAL_PERSON_ORGANIZATION ( #7097, #14387, #14360 ) ;
#11264 = CARTESIAN_POINT ( 'NONE',  ( 138.7771837325805393, -3662.202322998884483, 2257.629692227153555 ) ) ;
#11265 = PERSON_AND_ORGANIZATION ( #5446, #1895 ) ;
#11266 = ADVANCED_FACE ( 'NONE', ( #7477 ), #18025, .T. ) ;
#11267 = CARTESIAN_POINT ( 'NONE',  ( 9.855200508370408841, -3659.504995334291834, 2257.962940200996854 ) ) ;
#11268 = CARTESIAN_POINT ( 'NONE',  ( 9.920099014910965352, -3578.890613119102454, 2250.236564201333294 ) ) ;
#11269 = CARTESIAN_POINT ( 'NONE',  ( 10.36831320283000046, -3640.848700000000008, 2296.210799999999836 ) ) ;
#11270 = PRODUCT_DEFINITION_SHAPE ( 'NONE', 'NONE',  #23169 ) ;
#11271 = ADVANCED_FACE ( 'NONE', ( #16607 ), #18135, .F. ) ;
#11272 = CARTESIAN_POINT ( 'NONE',  ( 139.6999999999999886, -3574.034000000000106, 2245.359999999999673 ) ) ;
#11273 = AXIS2_PLACEMENT_3D ( 'NONE', #288, #167, #5443 ) ;
#11274 = EDGE_CURVE ( 'NONE', #13472, #8900, #10309, .T. ) ;
#11275 = ORIENTED_EDGE ( 'NONE', *, *, #18272, .T. ) ;
#11276 = CARTESIAN_POINT ( 'NONE',  ( 140.9395118823992448, -3662.065970330268556, 2249.485863044558755 ) ) ;
#11277 = ORIENTED_EDGE ( 'NONE', *, *, #12155, .T. ) ;
#11278 = APPROVAL_PERSON_ORGANIZATION ( #2686, #5473, #1045 ) ;
#11279 = VERTEX_POINT ( 'NONE', #21884 ) ;
#11280 = DIRECTION ( 'NONE',  ( 0.000000000000000000, 1.000000000000000000, 0.000000000000000000 ) ) ;
#11281 = ORIENTED_EDGE ( 'NONE', *, *, #7636, .T. ) ;
#11282 = DIRECTION ( 'NONE',  ( 0.5000000000040877302, 0.8660254037820785955, 0.000000000000000000 ) ) ;
#11283 = CONTEXT_DEPENDENT_SHAPE_REPRESENTATION ( #22064, #4160 ) ;
#11284 = DIRECTION ( 'NONE',  ( -1.000000000000000000, 0.000000000000000000, 0.000000000000000000 ) ) ;
#11285 = B_SPLINE_CURVE_WITH_KNOTS ( 'NONE', 3,
 ( #12825, #11064, #14246, #17981, #16345, #16227, #1817, #21627, #8740, #5226, #10725, #7441, #19511, #17871, #3453, #3686, #18099, #19754, #5690, #14363, #16000, #12604, #5579, #10608, #23129 ),
 .UNSPECIFIED., .F., .F.,
 ( 4, 2, 2, 2, 1, 2, 2, 2, 2, 1, 1, 2, 2, 4 ),
 ( 0.000000000000000000, 0.2500000000093751118, 0.3750000000138445921, 0.4375000000160857438, 0.4687500000172130643, 0.4843750000177767800, 0.5000000000183404403, 0.6250000000212408979, 0.6875000000222054597, 0.7187500000228344010, 0.7343750000228381758, 0.7421875000224096297, 0.7500000000219809726, 1.000000000000000000 ),
 .UNSPECIFIED. ) ;
#11286 = VECTOR ( 'NONE', #21164, 1000.000000000000000 ) ;
#11287 = EDGE_CURVE ( 'NONE', #20662, #19560, #7702, .T. ) ;
#11288 = EDGE_LOOP ( 'NONE', ( #2473, #15039, #12114, #10705 ) ) ;
#11289 = CARTESIAN_POINT ( 'NONE',  ( 7.021062793573091376, -3658.864052490032464, 2244.849304824781484 ) ) ;
#11290 = FACE_BOUND ( 'NONE', #6247, .T. ) ;
#11291 = DIRECTION ( 'NONE',  ( 1.000000000000000000, 0.000000000000000000, 0.000000000000000000 ) ) ;
#11292 = DIRECTION ( 'NONE',  ( 0.000000000000000000, 0.000000000000000000, 1.000000000000000000 ) ) ;
#11293 = COORDINATED_UNIVERSAL_TIME_OFFSET ( 0, 0, .AHEAD. ) ;
#11294 = DIRECTION ( 'NONE',  ( -0.000000000000000000, -1.000000000000000000, -0.000000000000000000 ) ) ;
#11295 = CARTESIAN_POINT ( 'NONE',  ( 151.4000000000000057, -3578.860000000000127, 2247.392000000000280 ) ) ;
#11296 = EDGE_CURVE ( 'NONE', #13554, #16048, #22661, .T. ) ;
#11297 = CARTESIAN_POINT ( 'NONE',  ( 22.22500000000000142, -3543.299999999999727, 2275.001800000000003 ) ) ;
#11298 = VERTEX_POINT ( 'NONE', #7370 ) ;
#11299 = AXIS2_PLACEMENT_3D ( 'NONE', #2612, #11294, #22287 ) ;
#11300 = DIRECTION ( 'NONE',  ( -0.7249994335945012525, 0.000000000000000000, 0.6887494619146010688 ) ) ;
#11301 = CARTESIAN_POINT ( 'NONE',  ( -0.7620000000000000107, -3660.140000000000327, 2244.547199999999975 ) ) ;
#11302 = ORIENTED_EDGE ( 'NONE', *, *, #20749, .F. ) ;
#11303 = DIRECTION ( 'NONE',  ( -1.000000000000000000, 0.000000000000000000, 0.000000000000000000 ) ) ;
#11304 = CARTESIAN_POINT ( 'NONE',  ( 18.28735818472415886, -3658.298849057980078, 2245.218321525803276 ) ) ;
#11305 = ORIENTED_EDGE ( 'NONE', *, *, #12436, .F. ) ;
#11306 = FACE_OUTER_BOUND ( 'NONE', #2036, .T. ) ;
#11307 = FACE_OUTER_BOUND ( 'NONE', #21960, .T. ) ;
#11308 = VECTOR ( 'NONE', #5371, 1000.000000000000000 ) ;
#11309 = FACE_OUTER_BOUND ( 'NONE', #917, .T. ) ;
#11310 = ADVANCED_FACE ( 'NONE', ( #19669 ), #11220, .F. ) ;
#11311 = CARTESIAN_POINT ( 'NONE',  ( -0.7620000000000000107, -3660.140000000000327, 2250.236800000000130 ) ) ;
#11312 = DIRECTION ( 'NONE',  ( 0.000000000000000000, 0.000000000000000000, -1.000000000000000000 ) ) ;
#11313 = AXIS2_PLACEMENT_3D ( 'NONE', #15912, #11802, #8412 ) ;
#11314 = AXIS2_PLACEMENT_3D ( 'NONE', #19832, #19724, #3536 ) ;
#11315 = CARTESIAN_POINT ( 'NONE',  ( 7.220772795361150465, -3577.865013798726068, 2244.723500464976496 ) ) ;
#11316 = ORIENTED_EDGE ( 'NONE', *, *, #12978, .F. ) ;
#11317 = COORDINATED_UNIVERSAL_TIME_OFFSET ( 0, 0, .AHEAD. ) ;
#11318 = VECTOR ( 'NONE', #21066, 1000.000000000000000 ) ;
#11319 = CARTESIAN_POINT ( 'NONE',  ( 61.26424768829000556, -3694.938000000000102, 2280.589800000000196 ) ) ;
#11320 = DIRECTION ( 'NONE',  ( 0.000000000000000000, 0.000000000000000000, -1.000000000000000000 ) ) ;
#11321 = CARTESIAN_POINT ( 'NONE',  ( 19.05000000000000071, -3578.860000000000127, 2247.392000000000280 ) ) ;
#11322 = ORIENTED_EDGE ( 'NONE', *, *, #19292, .T. ) ;
#11323 = CIRCLE ( 'NONE', #4581, 5.079999999999973426 ) ;
#11324 = CARTESIAN_POINT ( 'NONE',  ( 134.3616369522012235, -3661.583675183895139, 2244.919872097237203 ) ) ;
#11325 = APPLIED_PERSON_AND_ORGANIZATION_ASSIGNMENT ( #2686, #8092, ( #9761 ) ) ;
#11326 = EDGE_LOOP ( 'NONE', ( #2112, #950 ) ) ;
#11327 = CARTESIAN_POINT ( 'NONE',  ( 12.69999999999999929, -3579.494999999999891, 2239.771999999999935 ) ) ;
#11328 = ORIENTED_EDGE ( 'NONE', *, *, #4229, .F. ) ;
#11329 = VECTOR ( 'NONE', #12901, 1000.000000000000114 ) ;
#11330 = CARTESIAN_POINT ( 'NONE',  ( 14.02072516994395990, -3662.024738521661675, 2249.522943300878978 ) ) ;
#11331 = AXIS2_PLACEMENT_3D ( 'NONE', #430, #14731, #18346 ) ;
#11332 = DIRECTION ( 'NONE',  ( 0.000000000000000000, 0.000000000000000000, -1.000000000000000000 ) ) ;
#11333 = ORIENTED_EDGE ( 'NONE', *, *, #20734, .F. ) ;
#11334 = DIRECTION ( 'NONE',  ( 5.432398939370942693E-28, 1.000000000000000000, 2.336881798971000105E-14 ) ) ;
#11335 = FACE_OUTER_BOUND ( 'NONE', #14224, .T. ) ;
#11336 = ORIENTED_EDGE ( 'NONE', *, *, #8733, .F. ) ;
#11337 = DIRECTION ( 'NONE',  ( 0.000000000000000000, 0.000000000000000000, -1.000000000000000000 ) ) ;
#11338 = CARTESIAN_POINT ( 'NONE',  ( 139.6999999999999886, -3659.504999999999654, 2272.030000000000200 ) ) ;
#11339 = AXIS2_PLACEMENT_3D ( 'NONE', #10782, #17693, #7160 ) ;
#11340 = ORIENTED_EDGE ( 'NONE', *, *, #7864, .F. ) ;
#11341 = DIRECTION ( 'NONE',  ( 0.000000000000000000, 0.000000000000000000, -1.000000000000000000 ) ) ;
#11342 = UNCERTAINTY_MEASURE_WITH_UNIT (LENGTH_MEASURE( 1.000000000000000082E-05 ), #3304, 'distance_accuracy_value', 'NONE');
#11343 = ORIENTED_EDGE ( 'NONE', *, *, #214, .T. ) ;
#11345 = CARTESIAN_POINT ( 'NONE',  ( 12.69999999999999929, -3659.504999999999654, 2239.009999999999764 ) ) ;
#11344 = AXIS2_PLACEMENT_3D ( 'NONE', #13776, #20918, #4857 ) ;
#11346 = VECTOR ( 'NONE', #4817, 1000.000000000000000 ) ;
#11347 = DIRECTION ( 'NONE',  ( -1.000000000000000000, 0.000000000000000000, 0.000000000000000000 ) ) ;
#11348 = CARTESIAN_POINT ( 'NONE',  ( 18.03108505668890160, -3661.564694289580530, 2244.928212203581552 ) ) ;
#11349 = CARTESIAN_POINT ( 'NONE',  ( 15.41268679728753099, -3577.928829547073747, 2239.009999999999764 ) ) ;
#11350 = APPROVAL ( #20427, 'UNSPECIFIED' ) ;
#11351 = CARTESIAN_POINT ( 'NONE',  ( 11.12270644712000056, -3577.121901140999853, 2257.704293189000055 ) ) ;
#11352 = CARTESIAN_POINT ( 'NONE',  ( 137.2845969902833190, -3577.991942408667001, 2250.101189474289185 ) ) ;
#11353 = ORIENTED_EDGE ( 'NONE', *, *, #21324, .F. ) ;
#11354 = AXIS2_PLACEMENT_3D ( 'NONE', #19348, #12317, #8914 ) ;
#11355 = FACE_OUTER_BOUND ( 'NONE', #19470, .T. ) ;
#11356 = ADVANCED_FACE ( 'NONE', ( #2320 ), #5617, .F. ) ;
#11357 = EDGE_LOOP ( 'NONE', ( #11065, #2626 ) ) ;
#11358 = DIRECTION ( 'NONE',  ( 0.000000000000000000, 0.000000000000000000, -1.000000000000000000 ) ) ;
#11359 = ORIENTED_EDGE ( 'NONE', *, *, #21349, .F. ) ;
#11360 = ADVANCED_FACE ( 'NONE', ( #9006 ), #16155, .T. ) ;
#11361 = DIRECTION ( 'NONE',  ( -2.324635735433000053E-14, 0.000000000000000000, -1.000000000000000000 ) ) ;
#11362 = CARTESIAN_POINT ( 'NONE',  ( 139.6999999999999886, -3662.349799999999050, 2257.592639999999847 ) ) ;
#11363 = ADVANCED_FACE ( 'NONE', ( #13552 ), #21995, .T. ) ;
#11364 = VERTEX_POINT ( 'NONE', #11554 ) ;
#11365 = ORIENTED_EDGE ( 'NONE', *, *, #15101, .F. ) ;
#11366 = DIRECTION ( 'NONE',  ( 0.000000000000000000, -1.000000000000000000, 0.000000000000000000 ) ) ;
#11367 = ORIENTED_EDGE ( 'NONE', *, *, #11634, .F. ) ;
#11368 = CARTESIAN_POINT ( 'NONE',  ( 123.3932000000010021, -3568.700000000000273, 2260.600000000000364 ) ) ;
#11369 = CARTESIAN_POINT ( 'NONE',  ( 11.34078435016211017, -3576.994266383828744, 2249.540230614989923 ) ) ;
#11370 =( NAMED_UNIT ( * ) PLANE_ANGLE_UNIT ( ) SI_UNIT ( $, .RADIAN. ) );
#11371 = ADVANCED_FACE ( 'NONE', ( #6186 ), #1655, .T. ) ;
#11372 = CARTESIAN_POINT ( 'NONE',  ( 142.4707046595244435, -3580.142024907966061, 2249.931733785477263 ) ) ;
#11373 = ORIENTED_EDGE ( 'NONE', *, *, #21349, .T. ) ;
#11374 = CARTESIAN_POINT ( 'NONE',  ( 127.0000000000000000, -3578.860000000000127, 2250.236800000000130 ) ) ;
#11375 = APPROVAL_STATUS ( 'not_yet_approved' ) ;
#11376 = AXIS2_PLACEMENT_3D ( 'NONE', #19528, #8633, #10152 ) ;
#11377 = FACE_OUTER_BOUND ( 'NONE', #4815, .T. ) ;
#11378 = LINE ( 'NONE', #12797, #22147 ) ;
#11379 = EDGE_LOOP ( 'NONE', ( #18626, #18878, #14439, #20195, #4538 ) ) ;
#11380 = CARTESIAN_POINT ( 'NONE',  ( 20.54577294660182574, -3543.513261182326460, 2260.034604413234774 ) ) ;
#11381 = EDGE_CURVE ( 'NONE', #7352, #19931, #13094, .T. ) ;
#11382 = ADVANCED_FACE ( 'NONE', ( #16829 ), #13324, .T. ) ;
#11383 = ORIENTED_EDGE ( 'NONE', *, *, #4975, .T. ) ;
#11384 = FACE_OUTER_BOUND ( 'NONE', #22972, .T. ) ;
#11385 = ORIENTED_EDGE ( 'NONE', *, *, #2554, .T. ) ;
#11386 = ORIENTED_EDGE ( 'NONE', *, *, #13000, .F. ) ;
#11387 = AXIS2_PLACEMENT_3D ( 'NONE', #879, #13197, #18477 ) ;
#11389 = EDGE_CURVE ( 'NONE', #9827, #12111, #4260, .T. ) ;
#11388 = CIRCLE ( 'NONE', #21885, 5.080000000000000959 ) ;
#11390 = DIRECTION ( 'NONE',  ( 0.000000000000000000, 0.000000000000000000, -1.000000000000000000 ) ) ;
#11391 = VECTOR ( 'NONE', #4970, 999.9999999999998863 ) ;
#11392 = EDGE_LOOP ( 'NONE', ( #361, #22976, #6603, #21800, #10648 ) ) ;
#11393 = PLANE ( 'NONE',  #1549 ) ;
#11394 = CYLINDRICAL_SURFACE ( 'NONE', #3548, 0.7619999999999231832 ) ;
#11395 = ORIENTED_EDGE ( 'NONE', *, *, #18689, .F. ) ;
#11396 = CARTESIAN_POINT ( 'NONE',  ( 7.081767858629972601, -3658.457637283788245, 2245.097076080513034 ) ) ;
#11397 = CARTESIAN_POINT ( 'NONE',  ( 141.6126669512999854, -3657.399152860999493, 2246.630000000000109 ) ) ;
#11398 = DIRECTION ( 'NONE',  ( -1.000000000000000000, 0.000000000000000000, 0.000000000000000000 ) ) ;
#11399 = CARTESIAN_POINT ( 'NONE',  ( 142.0316867971999955, -3660.851200000000063, 2242.820000000000164 ) ) ;
#11400 = DATE_AND_TIME ( #4262, #14271 ) ;
#11401 = DIRECTION ( 'NONE',  ( 7.082568872520999671E-14, 2.590196616236000185E-13, 1.000000000000000000 ) ) ;
#11402 = VECTOR ( 'NONE', #6277, 1000.000000000000000 ) ;
#11403 = AXIS2_PLACEMENT_3D ( 'NONE', #4814, #7904, #8463 ) ;
#11404 = VECTOR ( 'NONE', #15460, 1000.000000000000000 ) ;
#11405 = CARTESIAN_POINT ( 'NONE',  ( 142.3916810111898883, -3658.582482988547326, 2249.773500813597366 ) ) ;
#11406 = CARTESIAN_POINT ( 'NONE',  ( 116.8400000000000034, -3694.430000000000291, 2244.547199999999975 ) ) ;
#11407 = AXIS2_PLACEMENT_3D ( 'NONE', #4473, #955, #16893 ) ;
#11408 = ORIENTED_EDGE ( 'NONE', *, *, #12414, .F. ) ;
#11409 = CARTESIAN_POINT ( 'NONE',  ( 7.238999999999998991, -3599.497499999999945, 2296.210799999999836 ) ) ;
#11410 = DIRECTION ( 'NONE',  ( 0.000000000000000000, 0.000000000000000000, -1.000000000000000000 ) ) ;
#11411 = ORIENTED_EDGE ( 'NONE', *, *, #15098, .T. ) ;
#11412 = CARTESIAN_POINT ( 'NONE',  ( 57.14999999999999858, -3568.700000000000273, 2244.547199999999975 ) ) ;
#11413 = CARTESIAN_POINT ( 'NONE',  ( 63.50000000000000000, -3594.099999999999909, 2261.869999999999891 ) ) ;
#11414 = ORIENTED_EDGE ( 'NONE', *, *, #4614, .T. ) ;
#11415 = ORIENTED_EDGE ( 'NONE', *, *, #21334, .F. ) ;
#11416 = CARTESIAN_POINT ( 'NONE',  ( 111.4552000000009997, -3594.099999999999909, 2261.869999999999891 ) ) ;
#11417 = CIRCLE ( 'NONE', #9195, 1.904999999999823501 ) ;
#11418 = CARTESIAN_POINT ( 'NONE',  ( 18.41499991942999870, -3579.495498070999474, 2244.618783703000190 ) ) ;
#11419 = TOROIDAL_SURFACE ( 'NONE', #1692, 3.606799999999999784, 0.7620000000000000107 ) ;
#11420 = CARTESIAN_POINT ( 'NONE',  ( 59.97894309125000234, -3694.430000000000291, 2175.874270430000252 ) ) ;
#11421 = CIRCLE ( 'NONE', #22640, 1.269999999999882334 ) ;
#11422 = ADVANCED_FACE ( 'NONE', ( #6766 ), #15667, .F. ) ;
#11423 = LINE ( 'NONE', #6286, #9702 ) ;
#11424 = CIRCLE ( 'NONE', #7309, 2.844799999999999773 ) ;
#11425 = CARTESIAN_POINT ( 'NONE',  ( 25.39999999999999858, -3670.300000000000182, 2259.837999999999738 ) ) ;
#11426 = CARTESIAN_POINT ( 'NONE',  ( 12.69999999999999929, -3597.592500000000200, 2263.571799999999712 ) ) ;
#11427 = EDGE_CURVE ( 'NONE', #14057, #15423, #2092, .T. ) ;
#11428 = DIRECTION ( 'NONE',  ( -1.000000000000000000, 0.000000000000000000, 0.000000000000000000 ) ) ;
#11429 = ORIENTED_EDGE ( 'NONE', *, *, #12407, .F. ) ;
#11430 = APPROVAL_STATUS ( 'not_yet_approved' ) ;
#11431 = DIRECTION ( 'NONE',  ( 1.000000000000000000, -2.590196616232000093E-13, 0.000000000000000000 ) ) ;
#11432 = EDGE_CURVE ( 'NONE', #309, #2778, #20059, .T. ) ;
#11433 = FACE_OUTER_BOUND ( 'NONE', #11545, .T. ) ;
#11434 = CARTESIAN_POINT ( 'NONE',  ( -12.31900000000000084, -3580.206200000000081, 2249.723686796999573 ) ) ;
#11435 = AXIS2_PLACEMENT_3D ( 'NONE', #22447, #20477, #4426 ) ;
#11436 = ORIENTED_EDGE ( 'NONE', *, *, #2274, .F. ) ;
#11437 = AXIS2_PLACEMENT_3D ( 'NONE', #8172, #20695, #6188 ) ;
#11438 = ADVANCED_FACE ( 'NONE', ( #13670 ), #20820, .F. ) ;
#11439 = CARTESIAN_POINT ( 'NONE',  ( 134.9016472537431639, -3662.609787423094076, 2245.979656123309724 ) ) ;
#11440 = CIRCLE ( 'NONE', #11828, 5.460999999999938126 ) ;
#11441 = EDGE_CURVE ( 'NONE', #21039, #1907, #907, .T. ) ;
#11442 = LINE ( 'NONE', #2543, #19261 ) ;
#11443 = ORIENTED_EDGE ( 'NONE', *, *, #11567, .T. ) ;
#11444 = CARTESIAN_POINT ( 'NONE',  ( 57.14999999999999858, -3695.699999999999818, 2251.506800000000112 ) ) ;
#11445 = AXIS2_PLACEMENT_3D ( 'NONE', #16573, #12947, #18332 ) ;
#11446 = CARTESIAN_POINT ( 'NONE',  ( 14.25469908642767969, -3661.887822319809402, 2249.636899428696324 ) ) ;
#11447 = CARTESIAN_POINT ( 'NONE',  ( 114.2999999999999972, -3594.099999999999909, 2259.837999999999738 ) ) ;
#11448 = ORIENTED_EDGE ( 'NONE', *, *, #3375, .F. ) ;
#11449 = VECTOR ( 'NONE', #19014, 1000.000000000000000 ) ;
#11450 = DIRECTION ( 'NONE',  ( 0.000000000000000000, 0.000000000000000000, -1.000000000000000000 ) ) ;
#11451 = B_SPLINE_CURVE_WITH_KNOTS ( 'NONE', 3,
 ( #5988, #11252, #18396, #7616, #2352, #18511, #18167, #16632, #702, #21803, #12897, #7854, #258, #590, #22024, #21583, #5538 ),
 .UNSPECIFIED., .F., .F.,
 ( 4, 1, 1, 1, 1, 1, 1, 1, 1, 1, 1, 1, 1, 1, 4 ),
 ( 5.006989608022782729E-06, 0.07142857142856999519, 0.1428571428570999946, 0.2142857142857000075, 0.2857142857143000203, 0.3571428571429000054, 0.4285714285713999594, 0.5000000000000000000, 0.5714285714286000406, 0.6428571428570999391, 0.7142857142856999797, 0.7857142857142999093, 0.8571428571429000609, 0.9285714285714000704, 1.000000000000000000 ),
 .UNSPECIFIED. ) ;
#11452 = FACE_BOUND ( 'NONE', #4471, .T. ) ;
#11453 = PLANE ( 'NONE',  #8945 ) ;
#11454 = DIRECTION ( 'NONE',  ( -1.000000000000000000, 0.000000000000000000, 0.000000000000000000 ) ) ;
#11455 = AXIS2_PLACEMENT_3D ( 'NONE', #2630, #20551, #9886 ) ;
#11456 = CIRCLE ( 'NONE', #12591, 0.7619999999999987894 ) ;
#11457 = ORIENTED_EDGE ( 'NONE', *, *, #22303, .T. ) ;
#11458 = CIRCLE ( 'NONE', #12595, 1.904999999999823501 ) ;
#11459 = DIRECTION ( 'NONE',  ( -0.5000000000043488546, -0.8660254037819278272, 0.000000000000000000 ) ) ;
#11460 = ORIENTED_EDGE ( 'NONE', *, *, #17519, .T. ) ;
#11461 = CARTESIAN_POINT ( 'NONE',  ( 145.3965142458158653, -3579.956683882830021, 2244.766317903402069 ) ) ;
#11462 = VECTOR ( 'NONE', #8245, 1000.000000000000000 ) ;
#11463 = COORDINATED_UNIVERSAL_TIME_OFFSET ( 0, 0, .AHEAD. ) ;
#11464 = CARTESIAN_POINT ( 'NONE',  ( 145.3892580085656050, -3578.952152314642262, 2244.548477537923191 ) ) ;
#11465 = DIRECTION ( 'NONE',  ( 0.000000000000000000, 0.000000000000000000, -1.000000000000000000 ) ) ;
#11466 = CARTESIAN_POINT ( 'NONE',  ( 15.54479972196000048, -3579.494990611520279, 2257.962943248000101 ) ) ;
#11467 = CARTESIAN_POINT ( 'NONE',  ( 142.4126867972053674, -3581.061170452544502, 2239.009999999999764 ) ) ;
#11468 = CARTESIAN_POINT ( 'NONE',  ( 138.3436566013999993, -3657.155744320999929, 2239.391000000000076 ) ) ;
#11469 = ORIENTED_EDGE ( 'NONE', *, *, #3609, .T. ) ;
#11470 = DIRECTION ( 'NONE',  ( 2.330758767201999921E-14, 1.000000000000000000, -5.460979050843892707E-28 ) ) ;
#11471 = VECTOR ( 'NONE', #9650, 1000.000000000000000 ) ;
#11472 = DIRECTION ( 'NONE',  ( 0.000000000000000000, 0.000000000000000000, 1.000000000000000000 ) ) ;
#11473 = ORIENTED_EDGE ( 'NONE', *, *, #10361, .T. ) ;
#11474 = DIRECTION ( 'NONE',  ( 1.000000000000000000, 0.000000000000000000, -1.224646799147353207E-16 ) ) ;
#11475 = VECTOR ( 'NONE', #12748, 1000.000000000000000 ) ;
#11476 = CARTESIAN_POINT ( 'NONE',  ( 15.59711802843494510, -3543.356150272710238, 2254.879006054897218 ) ) ;
#11477 = AXIS2_PLACEMENT_3D ( 'NONE', #22763, #21256, #8946 ) ;
#11478 = ORIENTED_EDGE ( 'NONE', *, *, #6722, .T. ) ;
#11479 = ORIENTED_EDGE ( 'NONE', *, *, #2138, .F. ) ;
#11480 = AXIS2_PLACEMENT_3D ( 'NONE', #16354, #19996, #3927 ) ;
#11481 = ORIENTED_EDGE ( 'NONE', *, *, #14233, .T. ) ;
#11482 = CARTESIAN_POINT ( 'NONE',  ( 131.7757523116999891, -3544.570000000000164, 2260.600000000000364 ) ) ;
#11483 = ORIENTED_EDGE ( 'NONE', *, *, #3771, .F. ) ;
#11484 = APPLIED_DATE_AND_TIME_ASSIGNMENT ( #22123, #21675, ( #15652 ) ) ;
#11485 = CARTESIAN_POINT ( 'NONE',  ( 10.36831320292846925, -3660.851200000039626, 2239.391000000000076 ) ) ;
#11486 = CARTESIAN_POINT ( 'NONE',  ( 12.96979589339266781, -3576.650406904108877, 2249.183810675842324 ) ) ;
#11487 = CARTESIAN_POINT ( 'NONE',  ( 142.5448000000000093, -3579.495004790000166, 2250.165035197999714 ) ) ;
#11488 = VERTEX_POINT ( 'NONE', #5472 ) ;
#11489 = CARTESIAN_POINT ( 'NONE',  ( 139.6999999999999886, -3662.349799999999050, 2257.592639999999847 ) ) ;
#11490 = APPLICATION_PROTOCOL_DEFINITION ( 'international standard', 'automotive_design', 2000, #18170 ) ;
#11491 = VECTOR ( 'NONE', #22375, 1000.000000000000000 ) ;
#11492 = EDGE_CURVE ( 'NONE', #724, #3211, #12149, .T. ) ;
#11493 = FACE_OUTER_BOUND ( 'NONE', #20314, .T. ) ;
#11494 = FACE_OUTER_BOUND ( 'NONE', #16090, .T. ) ;
#11495 = ADVANCED_FACE ( 'NONE', ( #12617 ), #11082, .F. ) ;
#11496 = DIRECTION ( 'NONE',  ( 0.000000000000000000, -1.000000000000000000, 0.000000000000000000 ) ) ;
#11497 = AXIS2_PLACEMENT_3D ( 'NONE', #4238, #4353, #16651 ) ;
#11498 = AXIS2_PLACEMENT_3D ( 'NONE', #20692, #7822, #15085 ) ;
#11499 = ORIENTED_EDGE ( 'NONE', *, *, #5806, .F. ) ;
#11500 = CARTESIAN_POINT ( 'NONE',  ( 142.0922539695508249, -3661.044633775621151, 2250.089196751532199 ) ) ;
#11501 = ORIENTED_EDGE ( 'NONE', *, *, #740, .T. ) ;
#11502 = ORIENTED_EDGE ( 'NONE', *, *, #14589, .F. ) ;
#11503 = AXIS2_PLACEMENT_3D ( 'NONE', #14389, #1734, #3709 ) ;
#11504 = CARTESIAN_POINT ( 'NONE',  ( 15.03168679707234467, -3600.843700000039007, 2296.210799999999836 ) ) ;
#11505 = ORIENTED_EDGE ( 'NONE', *, *, #10999, .T. ) ;
#11506 = DIRECTION ( 'NONE',  ( 0.000000000000000000, 0.000000000000000000, 1.000000000000000000 ) ) ;
#11507 = CARTESIAN_POINT ( 'NONE',  ( 63.50000000000000000, -3594.099999999999909, 2239.009999999999764 ) ) ;
#11508 = ORIENTED_EDGE ( 'NONE', *, *, #9724, .T. ) ;
#11509 = AXIS2_PLACEMENT_3D ( 'NONE', #15165, #2513, #20328 ) ;
#11510 = CARTESIAN_POINT ( 'NONE',  ( 22.55520000000100111, -3670.300000000000182, 2239.771999999999935 ) ) ;
#11511 = CARTESIAN_POINT ( 'NONE',  ( -6.349999999999999645, -3578.860000000000127, 2247.392000000000280 ) ) ;
#11512 = CARTESIAN_POINT ( 'NONE',  ( 88.90000000000000568, -3594.099999999999909, 2239.009999999999764 ) ) ;
#11513 = SHAPE_DEFINITION_REPRESENTATION ( #9215, #16547 ) ;
#11514 = EDGE_CURVE ( 'NONE', #4556, #309, #23139, .T. ) ;
#11515 = DIRECTION ( 'NONE',  ( 0.000000000000000000, 0.000000000000000000, -1.000000000000000000 ) ) ;
#11516 = EDGE_CURVE ( 'NONE', #10930, #16884, #22081, .T. ) ;
#11517 = CARTESIAN_POINT ( 'NONE',  ( 25.39999999999999858, -3619.500000000000000, 2239.771999999999935 ) ) ;
#11518 = EDGE_CURVE ( 'NONE', #2348, #5217, #5702, .T. ) ;
#11519 = EDGE_CURVE ( 'NONE', #8062, #17093, #10848, .T. ) ;
#11520 = CARTESIAN_POINT ( 'NONE',  ( 12.70000020906999971, -3662.349800009999854, 2257.592639999999847 ) ) ;
#11521 = AXIS2_PLACEMENT_3D ( 'NONE', #8363, #8823, #15501 ) ;
#11522 = CYLINDRICAL_SURFACE ( 'NONE', #15637, 2.844799999999999773 ) ;
#11523 = B_SPLINE_CURVE_WITH_KNOTS ( 'NONE', 3,
 ( #6242, #20300, #12916, #7875, #497, #4243, #15027, #13252, #4016, #828, #20405, #15137, #9512, #18303, #9408, #2259 ),
 .UNSPECIFIED., .F., .F.,
 ( 4, 2, 2, 2, 2, 2, 2, 4 ),
 ( 0.008925572905118884029, 0.009483443516259321138, 0.01004131412739975825, 0.01059918473854019536, 0.01115705534968063073, 0.01227279657196156393, 0.01283066718310207563, 0.01338853779424258733 ),
 .UNSPECIFIED. ) ;
#11524 = VERTEX_POINT ( 'NONE', #17761 ) ;
#11525 = DIRECTION ( 'NONE',  ( 0.000000000000000000, 1.000000000000000000, 0.000000000000000000 ) ) ;
#11526 = DIRECTION ( 'NONE',  ( 0.000000000000000000, -1.000000000000000000, 0.000000000000000000 ) ) ;
#11527 = VERTEX_POINT ( 'NONE', #5591 ) ;
#11528 = CARTESIAN_POINT ( 'NONE',  ( 50.79999999999999716, -3619.500000000000000, 2259.837999999999738 ) ) ;
#11529 = LINE ( 'NONE', #18677, #16280 ) ;
#11530 = ORIENTED_EDGE ( 'NONE', *, *, #7106, .T. ) ;
#11531 = EDGE_LOOP ( 'NONE', ( #2661, #4668, #14350, #14908 ) ) ;
#11532 = DIRECTION ( 'NONE',  ( -1.000000000000000000, 2.318894227180000040E-14, 2.343004830739999973E-14 ) ) ;
#11533 = CARTESIAN_POINT ( 'NONE',  ( 10.36831320285999958, -3578.148799999999937, 2242.820000000000164 ) ) ;
#11534 = CARTESIAN_POINT ( 'NONE',  ( 12.69999999999999929, -3659.504999999999654, 2239.009999999999764 ) ) ;
#11535 = DIRECTION ( 'NONE',  ( 1.000000000000000000, 0.000000000000000000, 0.000000000000000000 ) ) ;
#11536 = CARTESIAN_POINT ( 'NONE',  ( 12.69999999994000106, -3596.805100000000039, 2292.781800000000203 ) ) ;
#11537 = CIRCLE ( 'NONE', #708, 1.269999999999882334 ) ;
#11538 = DIRECTION ( 'NONE',  ( 0.000000000000000000, -1.000000000000000000, 0.000000000000000000 ) ) ;
#11539 = ORIENTED_EDGE ( 'NONE', *, *, #8213, .T. ) ;
#11540 = PERSON_AND_ORGANIZATION_ROLE ( 'classification_officer' ) ;
#11541 = LINE ( 'NONE', #20559, #2310 ) ;
#11542 = ADVANCED_FACE ( 'NONE', ( #12838 ), #5352, .T. ) ;
#11543 = DIRECTION ( 'NONE',  ( -1.000000000000000000, 0.000000000000000000, 0.000000000000000000 ) ) ;
#11544 = DIRECTION ( 'NONE',  ( -0.7249994335945980639, 0.000000000000000000, -0.6887494619144990393 ) ) ;
#11545 = EDGE_LOOP ( 'NONE', ( #16831, #5032, #442, #3080, #16616, #9188, #12453 ) ) ;
#11546 = FACE_OUTER_BOUND ( 'NONE', #3311, .T. ) ;
#11547 = ADVANCED_FACE ( 'NONE', ( #2184 ), #2064, .F. ) ;
#11548 = EDGE_CURVE ( 'NONE', #17616, #22650, #14030, .T. ) ;
#11549 = CYLINDRICAL_SURFACE ( 'NONE', #6167, 5.460999999999938126 ) ;
#11550 = CARTESIAN_POINT ( 'NONE',  ( 135.0294108980580177, -3576.200056266220145, 2246.372099701390198 ) ) ;
#11551 = ORIENTED_EDGE ( 'NONE', *, *, #8742, .T. ) ;
#11552 = AXIS2_PLACEMENT_3D ( 'NONE', #13183, #16589, #16921 ) ;
#11553 = CARTESIAN_POINT ( 'NONE',  ( 25.39999999999999858, -3619.500000000000000, 2259.837999999999738 ) ) ;
#11554 = CARTESIAN_POINT ( 'NONE',  ( 19.17699999999999960, -3579.494999999999891, 2239.009999999999764 ) ) ;
#11555 = APPLICATION_CONTEXT ( 'configuration controlled 3d designs of mechanical parts and assemblies' ) ;
#11556 = CARTESIAN_POINT ( 'NONE',  ( 142.0316867971268096, -3580.841200000091249, 2239.391000000000076 ) ) ;
#11557 = VERTEX_POINT ( 'NONE', #3810 ) ;
#11558 = ADVANCED_FACE ( 'NONE', ( #19997 ), #1946, .T. ) ;
#11559 = FACE_OUTER_BOUND ( 'NONE', #19955, .T. ) ;
#11560 = FACE_OUTER_BOUND ( 'NONE', #7063, .T. ) ;
#11561 = DIRECTION ( 'NONE',  ( -0.000000000000000000, -1.000000000000000000, -0.000000000000000000 ) ) ;
#11562 = CARTESIAN_POINT ( 'NONE',  ( 12.69999999999999929, -3642.677500000000236, 2264.841800000000148 ) ) ;
#11563 = ORIENTED_EDGE ( 'NONE', *, *, #21769, .F. ) ;
#11564 = ADVANCED_FACE ( 'NONE', ( #9329 ), #7226, .F. ) ;
#11565 = ORIENTED_EDGE ( 'NONE', *, *, #17290, .F. ) ;
#11566 = CIRCLE ( 'NONE', #11211, 3.606799999998994366 ) ;
#11567 = EDGE_CURVE ( 'NONE', #15816, #12211, #8792, .T. ) ;
#11568 = ORIENTED_EDGE ( 'NONE', *, *, #16887, .T. ) ;
#11569 = CIRCLE ( 'NONE', #22808, 3.606799999999993567 ) ;
#11570 = CARTESIAN_POINT ( 'NONE',  ( 20.32000000000000028, -3694.938000000000102, 2292.057900000000245 ) ) ;
#11571 = APPROVAL_DATE_TIME ( #2560, #6053 ) ;
#11572 = DIRECTION ( 'NONE',  ( 0.000000000000000000, 1.000000000000000000, 0.000000000000000000 ) ) ;
#11573 = CARTESIAN_POINT ( 'NONE',  ( 18.25703861352807067, -3660.839310627418854, 2244.634233714717993 ) ) ;
#11574 = LINE ( 'NONE', #14767, #16353 ) ;
#11575 = DIRECTION ( 'NONE',  ( 0.000000000000000000, -1.000000000000000000, 0.000000000000000000 ) ) ;
#11576 = EDGE_CURVE ( 'NONE', #4104, #20566, #7662, .T. ) ;
#11577 = CARTESIAN_POINT ( 'NONE',  ( 25.39999999999999858, -3619.500000000000000, 2260.600000000000364 ) ) ;
#11578 = ORIENTED_EDGE ( 'NONE', *, *, #7879, .F. ) ;
#11579 = DIRECTION ( 'NONE',  ( 0.000000000000000000, 0.000000000000000000, 1.000000000000000000 ) ) ;
#11580 = LINE ( 'NONE', #21434, #5847 ) ;
#11581 = EDGE_LOOP ( 'NONE', ( #49, #7910, #14975, #1600 ) ) ;
#11582 = LOCAL_TIME ( 17, 37, 43.00000000000000000, #16876 ) ;
#11583 = LINE ( 'NONE', #9828, #12538 ) ;
#11584 = CARTESIAN_POINT ( 'NONE',  ( 15.61212078344684251, -3543.344914976206383, 2254.841286577789560 ) ) ;
#11585 = ORIENTED_EDGE ( 'NONE', *, *, #9300, .F. ) ;
#11586 = ORIENTED_EDGE ( 'NONE', *, *, #16996, .F. ) ;
#11587 = ORIENTED_EDGE ( 'NONE', *, *, #6966, .T. ) ;
#11588 = CARTESIAN_POINT ( 'NONE',  ( 144.7800000000000011, -3579.494999999999891, 2239.391000000000076 ) ) ;
#11589 = ADVANCED_FACE ( 'NONE', ( #19638 ), #3582, .F. ) ;
#11590 = VERTEX_POINT ( 'NONE', #4159 ) ;
#11591 = LINE ( 'NONE', #20285, #10380 ) ;
#11592 = CARTESIAN_POINT ( 'NONE',  ( 11.14473204099212467, -3577.112510630018278, 2249.637028564206048 ) ) ;
#11593 = PRODUCT_CONTEXT ( 'NONE', #6788, 'mechanical' ) ;
#11594 = CARTESIAN_POINT ( 'NONE',  ( 141.9827405993179923, -3581.193534353457835, 2249.021006492486322 ) ) ;
#11595 = ORIENTED_EDGE ( 'NONE', *, *, #2260, .F. ) ;
#11596 = DIRECTION ( 'NONE',  ( 0.000000000000000000, 0.000000000000000000, 1.000000000000000000 ) ) ;
#11597 = APPROVAL_STATUS ( 'not_yet_approved' ) ;
#11598 = AXIS2_PLACEMENT_3D ( 'NONE', #550, #18356, #18245 ) ;
#11599 = CARTESIAN_POINT ( 'NONE',  ( 12.69999999999999929, -3599.497499999999945, 2263.571799999999712 ) ) ;
#11600 = ORGANIZATION ( 'NAUO-ORG3', 'UNSPECIFIED', 'UNSPECIFIED' ) ;
#11601 = CARTESIAN_POINT ( 'NONE',  ( 15.47291618100999955, -3660.140271294999820, 2250.236802488000194 ) ) ;
#11602 = LOCAL_TIME ( 17, 37, 43.00000000000000000, #20347 ) ;
#11603 = CARTESIAN_POINT ( 'NONE',  ( 12.69999999999999929, -3648.710000000000036, 2262.355140000000119 ) ) ;
#11604 = ORIENTED_EDGE ( 'NONE', *, *, #20736, .T. ) ;
#11605 = LINE ( 'NONE', #6358, #1723 ) ;
#11606 = APPLIED_PERSON_AND_ORGANIZATION_ASSIGNMENT ( #20197, #18861, ( #2304 ) ) ;
#11607 = ORIENTED_EDGE ( 'NONE', *, *, #17983, .T. ) ;
#11608 = ORIENTED_EDGE ( 'NONE', *, *, #3357, .F. ) ;
#11609 = FACE_OUTER_BOUND ( 'NONE', #11581, .T. ) ;
#11610 = VERTEX_POINT ( 'NONE', #7906 ) ;
#11611 = LOCAL_TIME ( 17, 37, 43.00000000000000000, #1448 ) ;
#11612 = FACE_OUTER_BOUND ( 'NONE', #8832, .T. ) ;
#11613 = DIRECTION ( 'NONE',  ( 0.8660254037820102058, -0.5000000000042060799, 0.000000000000000000 ) ) ;
#11614 = APPLIED_APPROVAL_ASSIGNMENT ( #21262, ( #3761 ) ) ;
#11615 = ORIENTED_EDGE ( 'NONE', *, *, #11677, .T. ) ;
#11616 = AXIS2_PLACEMENT_3D ( 'NONE', #17104, #10511, #15353 ) ;
#11617 = DIRECTION ( 'NONE',  ( 1.000000000000000000, 0.000000000000000000, 0.000000000000000000 ) ) ;
#11618 = DIRECTION ( 'NONE',  ( -1.000000000000000000, 1.224646799147353207E-16, 0.000000000000000000 ) ) ;
#11619 = FACE_OUTER_BOUND ( 'NONE', #8255, .T. ) ;
#11620 = PERSON_AND_ORGANIZATION ( #5446, #1895 ) ;
#11621 = AXIS2_PLACEMENT_3D ( 'NONE', #14809, #8954, #13048 ) ;
#11622 = DIRECTION ( 'NONE',  ( -1.000000000000000000, 0.000000000000000000, 0.000000000000000000 ) ) ;
#11623 = CARTESIAN_POINT ( 'NONE',  ( 25.39999999999999858, -3670.300000000000182, 2259.837999999999738 ) ) ;
#11624 = FACE_OUTER_BOUND ( 'NONE', #3873, .T. ) ;
#11625 = CARTESIAN_POINT ( 'NONE',  ( 0.000000000000000000, -3694.938000000000102, 2295.829799999999977 ) ) ;
#11626 = EDGE_LOOP ( 'NONE', ( #10362, #1769, #17510, #17339, #6331 ) ) ;
#11627 = CARTESIAN_POINT ( 'NONE',  ( 15.54478936534684941, -3659.505023738319323, 2250.165136749944850 ) ) ;
#11628 = APPLIED_DATE_AND_TIME_ASSIGNMENT ( #8267, #15529, ( #5365 ) ) ;
#11629 = VERTEX_POINT ( 'NONE', #2734 ) ;
#11630 = AXIS2_PLACEMENT_3D ( 'NONE', #20233, #20128, #15075 ) ;
#11631 = CARTESIAN_POINT ( 'NONE',  ( 142.5447999999989861, -3579.683680193961209, 2257.962944264955695 ) ) ;
#11632 = TOROIDAL_SURFACE ( 'NONE', #22496, 3.606799999999999784, 0.7620000000000000107 ) ;
#11633 = CARTESIAN_POINT ( 'NONE',  ( 18.37010631093954061, -3658.790234407184471, 2244.887790217552265 ) ) ;
#11634 = EDGE_CURVE ( 'NONE', #9357, #11488, #22234, .T. ) ;
#11635 = ORIENTED_EDGE ( 'NONE', *, *, #21305, .F. ) ;
#11636 = ORIENTED_EDGE ( 'NONE', *, *, #18297, .F. ) ;
#11637 = CARTESIAN_POINT ( 'NONE',  ( -6.730999999999880856, -3660.140000000000327, 2252.472000000000207 ) ) ;
#11638 = ADVANCED_FACE ( 'NONE', ( #16577 ), #10642, .T. ) ;
#11639 = CARTESIAN_POINT ( 'NONE',  ( 12.70000000000865903, -3582.187400000168964, 2239.167815367317871 ) ) ;
#11640 = CARTESIAN_POINT ( 'NONE',  ( 76.20000000000000284, -3670.300000000000182, 2259.837999999999738 ) ) ;
#11641 = EDGE_CURVE ( 'NONE', #3849, #20079, #6155, .T. ) ;
#11642 = DIRECTION ( 'NONE',  ( 0.000000000000000000, 0.000000000000000000, -1.000000000000000000 ) ) ;
#11643 = CARTESIAN_POINT ( 'NONE',  ( 142.2400000000000091, -3578.213872745999652, 2255.774000000000342 ) ) ;
#11644 = CARTESIAN_POINT ( 'NONE',  ( 136.8737869869528936, -3659.129981997597952, 2257.957971611072026 ) ) ;
#11645 = CARTESIAN_POINT ( 'NONE',  ( -6.349999999999999645, -3660.140000000000327, 2247.392000000000280 ) ) ;
#11646 = EDGE_LOOP ( 'NONE', ( #3838, #4736, #17535, #8835 ) ) ;
#11647 = PERSON_AND_ORGANIZATION_ROLE ( 'classification_officer' ) ;
#11648 = ORIENTED_EDGE ( 'NONE', *, *, #8263, .F. ) ;
#11649 = ADVANCED_FACE ( 'NONE', ( #9664 ), #646, .F. ) ;
#11650 = CARTESIAN_POINT ( 'NONE',  ( 145.2383954616615256, -3658.097948180692583, 2245.407198740987951 ) ) ;
#11651 = AXIS2_PLACEMENT_3D ( 'NONE', #20972, #4800, #8667 ) ;
#11652 = CARTESIAN_POINT ( 'NONE',  ( 12.69999999999999929, -3639.502500000000055, 2281.351799999999912 ) ) ;
#11653 = DIRECTION ( 'NONE',  ( 0.000000000000000000, 0.000000000000000000, -1.000000000000000000 ) ) ;
#11654 = ADVANCED_FACE ( 'NONE', ( #17029 ), #8024, .T. ) ;
#11655 = EDGE_LOOP ( 'NONE', ( #15097, #11501, #1175, #17613 ) ) ;
#11656 = DIRECTION ( 'NONE',  ( -1.000000000000000000, 0.000000000000000000, 0.000000000000000000 ) ) ;
#11657 = DIRECTION ( 'NONE',  ( 0.000000000000000000, -1.000000000000000000, 0.000000000000000000 ) ) ;
#11658 = CARTESIAN_POINT ( 'NONE',  ( 145.3796772601000100, -3660.139769217999856, 2244.548186305999934 ) ) ;
#11659 = ORIENTED_EDGE ( 'NONE', *, *, #8301, .F. ) ;
#11660 = LINE ( 'NONE', #2545, #989 ) ;
#11661 = TOROIDAL_SURFACE ( 'NONE', #10563, 4.114799999999999791, 1.270000000000000018 ) ;
#11662 = CARTESIAN_POINT ( 'NONE',  ( 14.54506894740048750, -3661.670460155497949, 2249.790026138201029 ) ) ;
#11663 = DIRECTION ( 'NONE',  ( -1.000000000000000000, 0.000000000000000000, 0.000000000000000000 ) ) ;
#11664 = VERTEX_POINT ( 'NONE', #6042 ) ;
#11665 = CIRCLE ( 'NONE', #9854, 5.079999999999973426 ) ;
#11666 = DIRECTION ( 'NONE',  ( 1.000000000000000000, 0.000000000000000000, 0.000000000000000000 ) ) ;
#11667 = CIRCLE ( 'NONE', #20653, 2.844800000000091700 ) ;
#11668 = LINE ( 'NONE', #22569, #16673 ) ;
#11669 = EDGE_CURVE ( 'NONE', #8539, #1092, #11388, .T. ) ;
#11670 = VECTOR ( 'NONE', #8638, 1000.000000000000000 ) ;
#11671 = DIRECTION ( 'NONE',  ( -1.000000000000000000, 0.000000000000000000, 0.000000000000000000 ) ) ;
#11672 = DIRECTION ( 'NONE',  ( 0.8660254037825932949, 0.5000000000031962211, 0.000000000000000000 ) ) ;
#11673 = DIRECTION ( 'NONE',  ( 0.000000000000000000, 0.000000000000000000, -1.000000000000000000 ) ) ;
#11674 = ORIENTED_EDGE ( 'NONE', *, *, #3981, .T. ) ;
#11675 = ORIENTED_EDGE ( 'NONE', *, *, #22609, .T. ) ;
#11676 = ADVANCED_FACE ( 'NONE', ( #13519 ), #9439, .T. ) ;
#11677 = EDGE_CURVE ( 'NONE', #4249, #14725, #13289, .T. ) ;
#11678 = FACE_OUTER_BOUND ( 'NONE', #10201, .T. ) ;
#11679 = ORIENTED_EDGE ( 'NONE', *, *, #269, .T. ) ;
#11680 = CARTESIAN_POINT ( 'NONE',  ( 15.33658054938999982, -3580.575448001000041, 2257.909769185999721 ) ) ;
#11682 = AXIS2_PLACEMENT_3D ( 'NONE', #12574, #17957, #8943 ) ;
#11681 = SECURITY_CLASSIFICATION_LEVEL ( 'unclassified' ) ;
#11683 = DIRECTION ( 'NONE',  ( 0.000000000000000000, 0.000000000000000000, 1.000000000000000000 ) ) ;
#11684 = CYLINDRICAL_SURFACE ( 'NONE', #6981, 2.844799999999999773 ) ;
#11685 = B_SPLINE_CURVE_WITH_KNOTS ( 'NONE', 3,
 ( #18681, #17034, #6392, #11418 ),
 .UNSPECIFIED., .F., .F.,
 ( 4, 4 ),
 ( 0.000000000000000000, 1.000000000000000000 ),
 .UNSPECIFIED. ) ;
#11686 = AXIS2_PLACEMENT_3D ( 'NONE', #7570, #16473, #21645 ) ;
#11687 = CARTESIAN_POINT ( 'NONE',  ( 13.51849986531999903, -3656.775770755999929, 2257.621751478000078 ) ) ;
#11688 = CARTESIAN_POINT ( 'NONE',  ( 116.8400000000000034, -3670.300000000000182, 2247.392000000000280 ) ) ;
#11689 = VECTOR ( 'NONE', #7917, 1000.000000000000000 ) ;
#11690 =( REPRESENTATION_RELATIONSHIP ('NONE','NONE', #20448, #7730 ) REPRESENTATION_RELATIONSHIP_WITH_TRANSFORMATION ( #459 )SHAPE_REPRESENTATION_RELATIONSHIP( ) );
#11691 = CYLINDRICAL_SURFACE ( 'NONE', #524, 0.3809999999999180154 ) ;
#11692 = ORIENTED_EDGE ( 'NONE', *, *, #16114, .F. ) ;
#11693 = EDGE_CURVE ( 'NONE', #17073, #6769, #3527, .T. ) ;
#11694 = DIRECTION ( 'NONE',  ( 0.000000000000000000, 0.000000000000000000, -1.000000000000000000 ) ) ;
#11695 = CIRCLE ( 'NONE', #14716, 2.844800000000001550 ) ;
#11696 = CARTESIAN_POINT ( 'NONE',  ( 92.50679999999999836, -3644.899999999999636, 2239.009999999999764 ) ) ;
#11697 = ORIENTED_EDGE ( 'NONE', *, *, #12880, .T. ) ;
#11698 = CARTESIAN_POINT ( 'NONE',  ( -12.31900000000000084, -3580.206200000000081, 2245.060313203000078 ) ) ;
#11699 = DIRECTION ( 'NONE',  ( 1.000000000000000000, 0.000000000000000000, 0.000000000000000000 ) ) ;
#11700 = VECTOR ( 'NONE', #18722, 1000.000000000000000 ) ;
#11701 = ORIENTED_EDGE ( 'NONE', *, *, #23005, .T. ) ;
#11702 = EDGE_LOOP ( 'NONE', ( #8658, #12875, #5910, #10820 ) ) ;
#11703 = ORIENTED_EDGE ( 'NONE', *, *, #337, .F. ) ;
#11704 = CARTESIAN_POINT ( 'NONE',  ( -12.31900000000001505, -3577.513799999857383, 2249.723686796824950 ) ) ;
#11705 = CIRCLE ( 'NONE', #12105, 5.460999999999938126 ) ;
#11706 = VERTEX_POINT ( 'NONE', #15059 ) ;
#11707 = EDGE_CURVE ( 'NONE', #4269, #21855, #3063, .T. ) ;
#11708 = CLOSED_SHELL ( 'NONE', ( #11155, #1488, #6128, #11271, #11166, #21276, #15945, #18790, #3502, #22445, #5239, #10866 ) ) ;
#11709 = DIRECTION ( 'NONE',  ( 1.000000000000000000, 0.000000000000000000, 2.117363008798000070E-13 ) ) ;
#11710 = EDGE_CURVE ( 'NONE', #17497, #8599, #13260, .T. ) ;
#11711 = CARTESIAN_POINT ( 'NONE',  ( 10.28467484152444200, -3577.991815362053330, 2250.101148760488741 ) ) ;
#11712 = DIRECTION ( 'NONE',  ( 0.000000000000000000, 0.000000000000000000, 1.000000000000000000 ) ) ;
#11713 = EDGE_CURVE ( 'NONE', #19144, #5409, #6227, .T. ) ;
#11714 = CARTESIAN_POINT ( 'NONE',  ( 141.7756668328444505, -3581.440556889209802, 2248.589885061244786 ) ) ;
#11715 = ORIENTED_EDGE ( 'NONE', *, *, #22391, .F. ) ;
#11716 = CARTESIAN_POINT ( 'NONE',  ( 137.4378580870267967, -3661.239941674269176, 2257.824813639031163 ) ) ;
#11717 = PERSON_AND_ORGANIZATION ( #5446, #1895 ) ;
#11718 = CARTESIAN_POINT ( 'NONE',  ( 116.8400000000000034, -3670.300000000000182, 2250.236800000000130 ) ) ;
#11719 = DIRECTION ( 'NONE',  ( 0.000000000000000000, 0.000000000000000000, -1.000000000000000000 ) ) ;
#11720 = EDGE_CURVE ( 'NONE', #13851, #6279, #22411, .T. ) ;
#11721 = AXIS2_PLACEMENT_3D ( 'NONE', #3097, #1103, #16077 ) ;
#11722 = CARTESIAN_POINT ( 'NONE',  ( 15.41268679713999923, -3601.063670452857423, 2296.591799999999694 ) ) ;
#11723 = AXIS2_PLACEMENT_3D ( 'NONE', #22086, #14957, #8154 ) ;
#11724 = ORIENTED_EDGE ( 'NONE', *, *, #10291, .T. ) ;
#11725 = FACE_OUTER_BOUND ( 'NONE', #7509, .T. ) ;
#11726 = EDGE_CURVE ( 'NONE', #1446, #12415, #12904, .T. ) ;
#11727 = AXIS2_PLACEMENT_3D ( 'NONE', #16184, #19709, #19822 ) ;
#11728 =( REPRESENTATION_RELATIONSHIP ('NONE','NONE', #20448, #6985 ) REPRESENTATION_RELATIONSHIP_WITH_TRANSFORMATION ( #2782 )SHAPE_REPRESENTATION_RELATIONSHIP( ) );
#11729 = ADVANCED_FACE ( 'NONE', ( #18908 ), #10791, .F. ) ;
#11730 = ORIENTED_EDGE ( 'NONE', *, *, #14955, .T. ) ;
#11731 = ORIENTED_EDGE ( 'NONE', *, *, #9104, .T. ) ;
#11732 = CARTESIAN_POINT ( 'NONE',  ( -5.588000000000000078, -3544.061999999999898, 2229.612000000000080 ) ) ;
#11733 = ORIENTED_EDGE ( 'NONE', *, *, #13960, .F. ) ;
#11734 = FACE_OUTER_BOUND ( 'NONE', #18541, .T. ) ;
#11735 = B_SPLINE_CURVE_WITH_KNOTS ( 'NONE', 3,
 ( #22648, #19031, #2970, #6624, #11882, #1775, #19585, #14433, #4733, #8919, #10117, #17931, #14202, #10561, #20782, #19708, #17700, #17261, #12431, #17148, #16064, #1647, #3519, #8805 ),
 .UNSPECIFIED., .F., .F.,
 ( 4, 2, 2, 1, 1, 1, 2, 2, 2, 2, 1, 2, 2, 4 ),
 ( 0.000000000000000000, 0.1249999999999866773, 0.1875000000002543799, 0.2187499999999581168, 0.2343749999998102629, 0.2421874999995853595, 0.2460937499996319056, 0.2499999999996784517, 0.3749999999999907296, 0.4375000000003181899, 0.4687500000004818923, 0.4843750000003246847, 0.5000000000001674216, 1.000000000000000000 ),
 .UNSPECIFIED. ) ;
#11736 = VECTOR ( 'NONE', #21548, 1000.000000000000000 ) ;
#11737 = VERTEX_POINT ( 'NONE', #13764 ) ;
#11738 = CARTESIAN_POINT ( 'NONE',  ( 7.259347590869622557, -3657.755355890642932, 2245.840513791162266 ) ) ;
#11739 = DIRECTION ( 'NONE',  ( 2.339144844575037611E-14, 0.000000000000000000, 1.000000000000000000 ) ) ;
#11740 = DIRECTION ( 'NONE',  ( -1.000000000000000000, 0.000000000000000000, 0.000000000000000000 ) ) ;
#11741 = APPROVAL_STATUS ( 'not_yet_approved' ) ;
#11742 = LINE ( 'NONE', #22518, #2831 ) ;
#11743 = CARTESIAN_POINT ( 'NONE',  ( 101.5999999999999943, -3568.700000000000273, 2239.771999999999935 ) ) ;
#11744 = VERTEX_POINT ( 'NONE', #19146 ) ;
#11745 = CYLINDRICAL_SURFACE ( 'NONE', #18634, 0.7619999999999294005 ) ;
#11746 =( BOUNDED_CURVE ( )  B_SPLINE_CURVE ( 3, ( #20005, #18233, #16133, #2194 ),
 .UNSPECIFIED., .F., .T. ) 
 B_SPLINE_CURVE_WITH_KNOTS ( ( 4, 4 ),
 ( 1.570796326441848079, 3.141592653589783346 ),
 .UNSPECIFIED. ) 
 CURVE ( )  GEOMETRIC_REPRESENTATION_ITEM ( )  RATIONAL_B_SPLINE_CURVE ( ( 1.000000000000000000, 0.8047378540411529446, 0.8047378540411529446, 1.000000000000000000 ) ) 
 REPRESENTATION_ITEM ( '' )  );
#11747 = CARTESIAN_POINT ( 'NONE',  ( 141.9904798895065312, -3657.817844140880425, 2249.035397113753334 ) ) ;
#11748 = FACE_OUTER_BOUND ( 'NONE', #10172, .T. ) ;
#11749 = ORIENTED_EDGE ( 'NONE', *, *, #16075, .T. ) ;
#11750 = LINE ( 'NONE', #739, #12616 ) ;
#11751 = EDGE_LOOP ( 'NONE', ( #22483, #18776, #18304, #4061, #4860 ) ) ;
#11752 = AXIS2_PLACEMENT_3D ( 'NONE', #8981, #7680, #20118 ) ;
#11753 = EDGE_LOOP ( 'NONE', ( #921, #6499, #22258, #8430, #18255, #7014, #17325 ) ) ;
#11754 = FACE_OUTER_BOUND ( 'NONE', #19274, .T. ) ;
#11755 = EDGE_LOOP ( 'NONE', ( #7381, #13421, #23032, #21501 ) ) ;
#11756 = ORIENTED_EDGE ( 'NONE', *, *, #3482, .T. ) ;
#11757 = CARTESIAN_POINT ( 'NONE',  ( 9.987313202864001482, -3581.061170452999704, 2239.009999999999764 ) ) ;
#11758 = DIRECTION ( 'NONE',  ( 0.000000000000000000, -1.000000000000000000, 0.000000000000000000 ) ) ;
#11759 = CARTESIAN_POINT ( 'NONE',  ( 9.866830068855998448, -3599.812301451999701, 2279.450423099000091 ) ) ;
#11760 = ORIENTED_EDGE ( 'NONE', *, *, #15973, .T. ) ;
#11761 = ORIENTED_EDGE ( 'NONE', *, *, #3952, .F. ) ;
#11762 = DIRECTION ( 'NONE',  ( 0.000000000000000000, 0.000000000000000000, 1.000000000000000000 ) ) ;
#11763 = FACE_OUTER_BOUND ( 'NONE', #11073, .T. ) ;
#11764 = CARTESIAN_POINT ( 'NONE',  ( 139.3259398483911013, -3656.678784355943208, 2257.597438744945066 ) ) ;
#11765 = CIRCLE ( 'NONE', #7660, 2.844800000000091700 ) ;
#11766 = DIRECTION ( 'NONE',  ( 0.000000000000000000, -1.000000000000000000, 0.000000000000000000 ) ) ;
#11767 = ORIENTED_EDGE ( 'NONE', *, *, #1701, .F. ) ;
#11768 = CALENDAR_DATE ( 2026, 26, 10 ) ;
#11769 = APPLIED_DATE_AND_TIME_ASSIGNMENT ( #18774, #4599, ( #381 ) ) ;
#11770 = AXIS2_PLACEMENT_3D ( 'NONE', #308, #9097, #14258 ) ;
#11771 = EDGE_CURVE ( 'NONE', #18027, #11171, #5810, .T. ) ;
#11772 = EDGE_LOOP ( 'NONE', ( #5729, #11054, #10751, #19149 ) ) ;
#11773 = CIRCLE ( 'NONE', #4666, 5.460999999999938126 ) ;
#11774 = CARTESIAN_POINT ( 'NONE',  ( -0.7620000000000000107, -3694.938000000000102, 2254.250000000000000 ) ) ;
#11775 = DIRECTION ( 'NONE',  ( 0.000000000000000000, -1.000000000000000000, 0.000000000000000000 ) ) ;
#11776 = EDGE_CURVE ( 'NONE', #4616, #3230, #14917, .T. ) ;
#11777 = CARTESIAN_POINT ( 'NONE',  ( 16.00573853068664931, -3543.299999999971988, 2281.667430734553363 ) ) ;
#11778 = EDGE_CURVE ( 'NONE', #16025, #5428, #16624, .T. ) ;
#11779 = ORIENTED_EDGE ( 'NONE', *, *, #17422, .F. ) ;
#11780 = ORIENTED_EDGE ( 'NONE', *, *, #2566, .T. ) ;
#11781 = DIRECTION ( 'NONE',  ( 0.000000000000000000, 0.000000000000000000, 1.000000000000000000 ) ) ;
#11782 = EDGE_CURVE ( 'NONE', #13993, #16307, #11735, .T. ) ;
#11783 = CIRCLE ( 'NONE', #2449, 2.844799999999999773 ) ;
#11784 = DIRECTION ( 'NONE',  ( 0.000000000000000000, -1.000000000000000000, 0.000000000000000000 ) ) ;
#11785 = CARTESIAN_POINT ( 'NONE',  ( 144.3705891021011780, -3662.799943733657074, 2246.372099701068237 ) ) ;
#11786 = ORIENTED_EDGE ( 'NONE', *, *, #12978, .T. ) ;
#11787 = DIRECTION ( 'NONE',  ( 1.000000000000000000, 0.000000000000000000, 0.000000000000000000 ) ) ;
#11788 = AXIS2_PLACEMENT_3D ( 'NONE', #20724, #15341, #22474 ) ;
#11789 = CARTESIAN_POINT ( 'NONE',  ( 14.86903996120028992, -3661.345726835937057, 2249.968664091575192 ) ) ;
#11790 = CIRCLE ( 'NONE', #1696, 2.844800000000091700 ) ;
#11791 = DIRECTION ( 'NONE',  ( 0.000000000000000000, 0.000000000000000000, -1.000000000000000000 ) ) ;
#11792 = AXIS2_PLACEMENT_3D ( 'NONE', #8350, #19359, #15491 ) ;
#11793 = ORIENTED_EDGE ( 'NONE', *, *, #4614, .F. ) ;
#11794 = ADVANCED_FACE ( 'NONE', ( #4613 ), #7288, .T. ) ;
#11795 = CARTESIAN_POINT ( 'NONE',  ( 141.6126318482000102, -3581.600863517000107, 2246.630000000000109 ) ) ;
#11796 = CARTESIAN_POINT ( 'NONE',  ( 13.01510790209967894, -3636.669354860410749, 2279.814648369741917 ) ) ;
#11797 = CARTESIAN_POINT ( 'NONE',  ( 133.9850000019999925, -3579.284332437912781, 2244.570779506149393 ) ) ;
#11798 = CYLINDRICAL_SURFACE ( 'NONE', #20324, 0.3810000000000260956 ) ;
#11799 = CARTESIAN_POINT ( 'NONE',  ( 114.2999999999999972, -3644.899999999999636, 2259.837999999999738 ) ) ;
#11800 = ORIENTED_EDGE ( 'NONE', *, *, #3541, .F. ) ;
#11801 = ORIENTED_EDGE ( 'NONE', *, *, #13804, .T. ) ;
#11802 = DIRECTION ( 'NONE',  ( 0.000000000000000000, 0.000000000000000000, 1.000000000000000000 ) ) ;
#11803 = AXIS2_PLACEMENT_3D ( 'NONE', #18601, #1124, #8057 ) ;
#11804 = ORIENTED_EDGE ( 'NONE', *, *, #12816, .T. ) ;
#11805 = CARTESIAN_POINT ( 'NONE',  ( 12.97541421502999981, -3582.330907204000141, 2257.594921553999939 ) ) ;
#11806 = TOROIDAL_SURFACE ( 'NONE', #21558, 6.477000000000000313, 0.7620000000000000107 ) ;
#11807 = CALENDAR_DATE ( 2026, 26, 10 ) ;
#11808 = CIRCLE ( 'NONE', #6593, 3.175000000000149925 ) ;
#11809 = ADVANCED_FACE ( 'NONE', ( #22530 ), #3641, .T. ) ;
#11810 = AXIS2_PLACEMENT_3D ( 'NONE', #1745, #15805, #22711 ) ;
#11811 = CARTESIAN_POINT ( 'NONE',  ( 142.5447999999989861, -3579.306313942341149, 2257.962944264954785 ) ) ;
#11812 = LINE ( 'NONE', #19200, #2843 ) ;
#11813 = EDGE_CURVE ( 'NONE', #7196, #18657, #8926, .T. ) ;
#11814 = CARTESIAN_POINT ( 'NONE',  ( 15.33662675678000120, -3658.424664496000332, 2257.909780506000061 ) ) ;
#11815 = EDGE_CURVE ( 'NONE', #2778, #3685, #8037, .T. ) ;
#11816 = FACE_OUTER_BOUND ( 'NONE', #22599, .T. ) ;
#11817 = CYLINDRICAL_SURFACE ( 'NONE', #9876, 0.3809999999999303388 ) ;
#11818 = ORIENTED_EDGE ( 'NONE', *, *, #5577, .F. ) ;
#11819 = DIRECTION ( 'NONE',  ( 1.000000000000000000, 0.000000000000000000, 0.000000000000000000 ) ) ;
#11820 = DIRECTION ( 'NONE',  ( 0.000000000000000000, 0.000000000000000000, -1.000000000000000000 ) ) ;
#11821 = ORIENTED_EDGE ( 'NONE', *, *, #8516, .T. ) ;
#11822 = TOROIDAL_SURFACE ( 'NONE', #1731, 3.606799999998999695, 0.7620000000000000107 ) ;
#11823 = VECTOR ( 'NONE', #15518, 1000.000000000000000 ) ;
#11824 = CYLINDRICAL_SURFACE ( 'NONE', #18519, 0.3810000000000746678 ) ;
#11825 = CARTESIAN_POINT ( 'NONE',  ( 10.66409421166686045, -3657.517533168687805, 2248.495888785344960 ) ) ;
#11826 = AXIS2_PLACEMENT_3D ( 'NONE', #9306, #7428, #7195 ) ;
#11827 = VERTEX_POINT ( 'NONE', #9277 ) ;
#11828 = AXIS2_PLACEMENT_3D ( 'NONE', #21424, #95, #14167 ) ;
#11829 = ORIENTED_EDGE ( 'NONE', *, *, #14188, .T. ) ;
#11830 = CARTESIAN_POINT ( 'NONE',  ( 134.3229528927292336, -3581.431939766277537, 2246.174326570847370 ) ) ;
#11831 = PRODUCT_DEFINITION_CONTEXT ( 'detailed design', #5277, 'design' ) ;
#11832 = ADVANCED_FACE ( 'NONE', ( #13020 ), #20375, .T. ) ;
#11833 = AXIS2_PLACEMENT_3D ( 'NONE', #16937, #11781, #1352 ) ;
#11834 = VERTEX_POINT ( 'NONE', #3749 ) ;
#11835 = CARTESIAN_POINT ( 'NONE',  ( 64.76999999999999602, -3568.700000000000273, 2286.368300000000090 ) ) ;
#11836 = CARTESIAN_POINT ( 'NONE',  ( 47.19319999999999737, -3568.700000000000273, 2239.771999999999935 ) ) ;
#11837 = CARTESIAN_POINT ( 'NONE',  ( 0.000000000000000000, 0.000000000000000000, 0.000000000000000000 ) ) ;
#11838 = VECTOR ( 'NONE', #23137, 1000.000000000000000 ) ;
#11839 = CARTESIAN_POINT ( 'NONE',  ( 142.1866385280289933, -3580.879155498138061, 2249.398837230915888 ) ) ;
#11840 = ORIENTED_EDGE ( 'NONE', *, *, #18859, .F. ) ;
#11841 = CARTESIAN_POINT ( 'NONE',  ( 131.8826821606740225, -3695.435514547667026, 2260.105825662819370 ) ) ;
#11842 = DATE_TIME_ROLE ( 'classification_date' ) ;
#11843 = DIRECTION ( 'NONE',  ( 0.6887494619146551367, 0.000000000000000000, -0.7249994335944497381 ) ) ;
#11844 = CARTESIAN_POINT ( 'NONE',  ( 14.78644416229590242, -3581.429898611652334, 2248.616548156125646 ) ) ;
#11845 = CARTESIAN_POINT ( 'NONE',  ( 134.2737407819179793, -3657.711383914624548, 2245.910523936043319 ) ) ;
#11846 = VECTOR ( 'NONE', #15457, 999.9999999999998863 ) ;
#11847 = ORIENTED_EDGE ( 'NONE', *, *, #18090, .T. ) ;
#11848 = VECTOR ( 'NONE', #6038, 1000.000000000000114 ) ;
#11849 = CARTESIAN_POINT ( 'NONE',  ( 142.1146155143981105, -3661.009309353270964, 2250.100788259126602 ) ) ;
#11850 = ADVANCED_FACE ( 'NONE', ( #5765 ), #3874, .T. ) ;
#11851 = EDGE_CURVE ( 'NONE', #749, #8027, #12522, .T. ) ;
#11852 = AXIS2_PLACEMENT_3D ( 'NONE', #5820, #3809, #13067 ) ;
#11853 = ORIENTED_EDGE ( 'NONE', *, *, #9859, .T. ) ;
#11854 = EDGE_CURVE ( 'NONE', #16863, #15415, #9494, .T. ) ;
#11855 = CARTESIAN_POINT ( 'NONE',  ( 25.39999999999999858, -3619.500000000000000, 2239.771999999999935 ) ) ;
#11856 = DIRECTION ( 'NONE',  ( -1.000000000000000000, 0.000000000000000000, 0.000000000000000000 ) ) ;
#11857 = ORIENTED_EDGE ( 'NONE', *, *, #20169, .F. ) ;
#11858 = VERTEX_POINT ( 'NONE', #2005 ) ;
#11859 = CARTESIAN_POINT ( 'NONE',  ( 63.50000000000000000, -3644.899999999999636, 2259.837999999999738 ) ) ;
#11860 = CARTESIAN_POINT ( 'NONE',  ( -5.588000000000000078, -3544.061999999999898, 2229.612000000000080 ) ) ;
#11861 = EDGE_CURVE ( 'NONE', #14115, #17865, #8406, .T. ) ;
#11862 = ORIENTED_EDGE ( 'NONE', *, *, #14260, .F. ) ;
#11863 = VECTOR ( 'NONE', #8477, 1000.000000000000000 ) ;
#11864 = DIRECTION ( 'NONE',  ( -0.5000000000047110094, -0.8660254037817188832, 0.000000000000000000 ) ) ;
#11865 = DIRECTION ( 'NONE',  ( 1.000000000000000000, 0.000000000000000000, 3.996303350731721563E-14 ) ) ;
#11866 = CARTESIAN_POINT ( 'NONE',  ( 12.80540748638105697, -3602.342302934895088, 2279.817638395105860 ) ) ;
#11867 = CARTESIAN_POINT ( 'NONE',  ( 95.25000000000000000, -3544.570000000000164, 2247.392000000000280 ) ) ;
#11868 = EDGE_CURVE ( 'NONE', #23061, #2750, #16758, .T. ) ;
#11869 = DATE_TIME_ROLE ( 'creation_date' ) ;
#11870 = ADVANCED_FACE ( 'NONE', ( #12780 ), #20164, .F. ) ;
#11871 = CIRCLE ( 'NONE', #7039, 2.844799999998998796 ) ;
#11872 = FACE_OUTER_BOUND ( 'NONE', #12587, .T. ) ;
#11873 = DIRECTION ( 'NONE',  ( 0.000000000000000000, -1.000000000000000000, 0.000000000000000000 ) ) ;
#11874 = DIRECTION ( 'NONE',  ( 1.000000000000000000, 0.000000000000000000, 0.000000000000000000 ) ) ;
#11875 = CARTESIAN_POINT ( 'NONE',  ( 142.0975596452481113, -3657.973835563076136, 2249.236080756626507 ) ) ;
#11876 = CARTESIAN_POINT ( 'NONE',  ( 20.32000000000000028, -3670.300000000000182, 2286.368300000000090 ) ) ;
#11877 = VERTEX_POINT ( 'NONE', #362 ) ;
#11878 = CARTESIAN_POINT ( 'NONE',  ( 137.1440651153584156, -3544.251379750218803, 2255.734039348538772 ) ) ;
#11879 = TOROIDAL_SURFACE ( 'NONE', #21983, 1.524000000000000021, 0.7620000000000000107 ) ;
#11880 = EDGE_CURVE ( 'NONE', #5789, #12735, #11451, .T. ) ;
#11881 = ORIENTED_EDGE ( 'NONE', *, *, #13941, .T. ) ;
#11882 = CARTESIAN_POINT ( 'NONE',  ( 4.722483775760038860, -3695.643849723204767, 2259.705165060028776 ) ) ;
#11883 = AXIS2_PLACEMENT_3D ( 'NONE', #18358, #18247, #14629 ) ;
#11884 = DIRECTION ( 'NONE',  ( 0.000000000000000000, 0.000000000000000000, -1.000000000000000000 ) ) ;
#11885 = AXIS2_PLACEMENT_3D ( 'NONE', #22151, #6238, #6123 ) ;
#11886 = ORIENTED_EDGE ( 'NONE', *, *, #22008, .T. ) ;
#11887 = ORIENTED_EDGE ( 'NONE', *, *, #12666, .T. ) ;
#11888 = B_SPLINE_CURVE_WITH_KNOTS ( 'NONE', 3,
 ( #15236, #9495, #16633, #591 ),
 .UNSPECIFIED., .F., .F.,
 ( 4, 4 ),
 ( 0.000000000000000000, 1.000000000000000000 ),
 .UNSPECIFIED. ) ;
#11889 = CARTESIAN_POINT ( 'NONE',  ( -12.31900000000000084, -3578.860000000000127, 2247.392000000000280 ) ) ;
#11890 = CARTESIAN_POINT ( 'NONE',  ( 12.69999999999999929, -3579.494999999999891, 2245.359999999999673 ) ) ;
#11891 = DIRECTION ( 'NONE',  ( -0.8660254037817187722, 0.5000000000047108983, 0.000000000000000000 ) ) ;
#11892 = ORIENTED_EDGE ( 'NONE', *, *, #16075, .F. ) ;
#11893 = CARTESIAN_POINT ( 'NONE',  ( 12.69999999999999929, -3659.504999999999654, 2239.391000000000076 ) ) ;
#11894 = DIRECTION ( 'NONE',  ( -1.000000000000000000, 0.000000000000000000, 0.000000000000000000 ) ) ;
#11895 = CARTESIAN_POINT ( 'NONE',  ( 35.56000000000000227, -3670.300000000000182, 2247.392000000000280 ) ) ;
#11896 = CARTESIAN_POINT ( 'NONE',  ( 136.8552000000010480, -3659.316319581317202, 2257.962944264956150 ) ) ;
#11897 = CARTESIAN_POINT ( 'NONE',  ( 20.54573065161225287, -3695.486738824718486, 2260.034587513629049 ) ) ;
#11898 = ORIENTED_EDGE ( 'NONE', *, *, #20562, .F. ) ;
#11899 = CALENDAR_DATE ( 2026, 26, 10 ) ;
#11900 = CIRCLE ( 'NONE', #9637, 0.7619999999999996776 ) ;
#11901 = VERTEX_POINT ( 'NONE', #20607 ) ;
#11902 = FACE_OUTER_BOUND ( 'NONE', #6994, .T. ) ;
#11903 = CARTESIAN_POINT ( 'NONE',  ( 10.22015228523534702, -3580.889289654939603, 2249.386560310950699 ) ) ;
#11904 = LINE ( 'NONE', #13312, #22412 ) ;
#11905 = ORIENTED_EDGE ( 'NONE', *, *, #9831, .T. ) ;
#11906 = ORIENTED_EDGE ( 'NONE', *, *, #21135, .T. ) ;
#11907 = FACE_BOUND ( 'NONE', #12619, .T. ) ;
#11908 = DIRECTION ( 'NONE',  ( 1.000000000000000000, 0.000000000000000000, 0.000000000000000000 ) ) ;
#11909 = CARTESIAN_POINT ( 'NONE',  ( 12.69999999999999929, -3639.502500000000055, 2296.591799999999694 ) ) ;
#11910 = DIRECTION ( 'NONE',  ( -1.000000000000000000, 0.000000000000000000, 0.000000000000000000 ) ) ;
#11911 = DIRECTION ( 'NONE',  ( -1.000000000000000000, 0.000000000000000000, 0.000000000000000000 ) ) ;
#11912 = APPROVAL ( #18184, 'UNSPECIFIED' ) ;
#11913 = DIRECTION ( 'NONE',  ( -1.000000000000000000, 0.000000000000000000, 0.000000000000000000 ) ) ;
#11914 = ORIENTED_EDGE ( 'NONE', *, *, #4937, .F. ) ;
#11915 = LINE ( 'NONE', #1244, #6152 ) ;
#11916 = CARTESIAN_POINT ( 'NONE',  ( 13.32717689757000024, -3636.721669530999861, 2279.801370455999859 ) ) ;
#11917 = EDGE_CURVE ( 'NONE', #19732, #4416, #2921, .T. ) ;
#11918 = DIRECTION ( 'NONE',  ( -1.000000000000000000, 0.000000000000000000, 0.000000000000000000 ) ) ;
#11919 = LINE ( 'NONE', #3008, #3467 ) ;
#11920 = FACE_OUTER_BOUND ( 'NONE', #5127, .T. ) ;
#11921 = ORIENTED_EDGE ( 'NONE', *, *, #16681, .T. ) ;
#11922 = ORIENTED_EDGE ( 'NONE', *, *, #1493, .F. ) ;
#11923 = EDGE_CURVE ( 'NONE', #3271, #15794, #5434, .T. ) ;
#11924 = EDGE_LOOP ( 'NONE', ( #5852, #3768, #13549, #7055 ) ) ;
#11925 = CARTESIAN_POINT ( 'NONE',  ( 12.69999999999999929, -3639.502500000000055, 2295.829799999999977 ) ) ;
#11926 = ORIENTED_EDGE ( 'NONE', *, *, #15885, .T. ) ;
#11927 = CARTESIAN_POINT ( 'NONE',  ( 13.51841762737000074, -3582.224253381999915, 2257.621745511999961 ) ) ;
#11928 = CARTESIAN_POINT ( 'NONE',  ( 97.99320000000000164, -3619.500000000000000, 2239.009999999999764 ) ) ;
#11929 = LINE ( 'NONE', #3021, #1125 ) ;
#11930 = DIRECTION ( 'NONE',  ( -1.000000000000000000, 0.000000000000000000, 0.000000000000000000 ) ) ;
#11931 = AXIS2_PLACEMENT_3D ( 'NONE', #15093, #7947, #4195 ) ;
#11932 = LINE ( 'NONE', #13579, #12979 ) ;
#11933 = CARTESIAN_POINT ( 'NONE',  ( 88.90000000000000568, -3644.899999999999636, 2239.771999999999935 ) ) ;
#11934 = PLANE ( 'NONE',  #887 ) ;
#11935 = ORIENTED_EDGE ( 'NONE', *, *, #10893, .T. ) ;
#11936 = CARTESIAN_POINT ( 'NONE',  ( 20.32000000000000028, -3568.700000000000273, 2292.057900000000245 ) ) ;
#11937 = APPLIED_PERSON_AND_ORGANIZATION_ASSIGNMENT ( #22314, #8036, ( #16119 ) ) ;
#11938 = DIRECTION ( 'NONE',  ( -1.000000000000000000, 0.000000000000000000, 0.000000000000000000 ) ) ;
#11939 = ORIENTED_EDGE ( 'NONE', *, *, #7426, .T. ) ;
#11940 = CARTESIAN_POINT ( 'NONE',  ( 18.40310581996000039, -3659.924389696708658, 2244.547177115724480 ) ) ;
#11941 = CARTESIAN_POINT ( 'NONE',  ( 10.87600349139550993, -3657.321675656191928, 2247.788763825722071 ) ) ;
#11942 = ORIENTED_EDGE ( 'NONE', *, *, #18146, .T. ) ;
#11943 = EDGE_CURVE ( 'NONE', #5168, #17725, #5059, .T. ) ;
#11944 = ORIENTED_EDGE ( 'NONE', *, *, #16521, .T. ) ;
#11945 = CARTESIAN_POINT ( 'NONE',  ( 22.55520000000100111, -3568.700000000000273, 2261.869999999999891 ) ) ;
#11946 = EDGE_CURVE ( 'NONE', #16187, #3108, #6150, .T. ) ;
#11947 = AXIS2_PLACEMENT_3D ( 'NONE', #11202, #2528, #2413 ) ;
#11948 = ORIENTED_EDGE ( 'NONE', *, *, #15747, .T. ) ;
#11949 = ADVANCED_FACE ( 'NONE', ( #7970 ), #8197, .F. ) ;
#11950 = CARTESIAN_POINT ( 'NONE',  ( 6.222999999999998977, -3639.502500000000055, 2295.829799999999977 ) ) ;
#11951 = CARTESIAN_POINT ( 'NONE',  ( 0.000000000000000000, 0.000000000000000000, 0.000000000000000000 ) ) ;
#11952 = FACE_OUTER_BOUND ( 'NONE', #21341, .T. ) ;
#11953 = ORIENTED_EDGE ( 'NONE', *, *, #2226, .T. ) ;
#11954 = CARTESIAN_POINT ( 'NONE',  ( 131.7444118345384823, -3695.625189109597613, 2259.759456293023959 ) ) ;
#11955 = PERSON_AND_ORGANIZATION_ROLE ( 'design_owner' ) ;
#11956 = LINE ( 'NONE', #8455, #20132 ) ;
#11957 = CARTESIAN_POINT ( 'NONE',  ( 15.31352823294669996, -3580.622497904614647, 2249.627690351728688 ) ) ;
#11958 = VECTOR ( 'NONE', #3395, 1000.000000000000000 ) ;
#11959 = CARTESIAN_POINT ( 'NONE',  ( 134.0820746908595140, -3658.455984731507215, 2245.098290645206362 ) ) ;
#11960 = APPLIED_APPROVAL_ASSIGNMENT ( #17646, ( #12365 ) ) ;
#11961 = ADVANCED_FACE ( 'NONE', ( #15118 ), #4307, .T. ) ;
#11962 = VERTEX_POINT ( 'NONE', #3032 ) ;
#11963 = CIRCLE ( 'NONE', #19445, 2.844800000000091700 ) ;
#11964 = CARTESIAN_POINT ( 'NONE',  ( 15.61261851050921479, -3695.655085023901847, 2254.841485307673338 ) ) ;
#11965 = CARTESIAN_POINT ( 'NONE',  ( 19.05000000000000071, -3582.035000000000309, 2247.392000000000280 ) ) ;
#11966 = EDGE_LOOP ( 'NONE', ( #5966, #659, #11697, #6743, #17117, #6825, #13568, #11578 ) ) ;
#11967 = CARTESIAN_POINT ( 'NONE',  ( 63.50000000000000000, -3594.099999999999909, 2259.837999999999738 ) ) ;
#11968 = CARTESIAN_POINT ( 'NONE',  ( 137.3683132029000262, -3578.148799999999937, 2239.391000000000076 ) ) ;
#11969 = ORIENTED_EDGE ( 'NONE', *, *, #12407, .T. ) ;
#11970 = ORIENTED_EDGE ( 'NONE', *, *, #5162, .F. ) ;
#11971 = DIRECTION ( 'NONE',  ( -1.000000000000000000, 0.000000000000000000, 0.000000000000000000 ) ) ;
#11972 = PLANE ( 'NONE',  #20778 ) ;
#11973 = CIRCLE ( 'NONE', #22089, 2.844799999999994444 ) ;
#11974 = VERTEX_POINT ( 'NONE', #8315 ) ;
#11975 = EDGE_CURVE ( 'NONE', #1715, #21296, #13231, .T. ) ;
#11976 = FACE_BOUND ( 'NONE', #9714, .T. ) ;
#11977 = DIRECTION ( 'NONE',  ( 0.000000000000000000, -1.000000000000000000, 0.000000000000000000 ) ) ;
#11978 = CARTESIAN_POINT ( 'NONE',  ( 15.27310817925000030, -3600.724796071000128, 2279.515941249000207 ) ) ;
#11979 = APPROVAL_PERSON_ORGANIZATION ( #22491, #8051, #13478 ) ;
#11980 =( GEOMETRIC_REPRESENTATION_CONTEXT ( 3 ) GLOBAL_UNCERTAINTY_ASSIGNED_CONTEXT ( ( #20261 ) ) GLOBAL_UNIT_ASSIGNED_CONTEXT ( ( #17013, #12678, #7291 ) ) REPRESENTATION_CONTEXT ( 'NONE', 'WORKASPACE' ) );
#11981 = LINE ( 'NONE', #20769, #4734 ) ;
#11982 = APPROVAL_DATE_TIME ( #8237, #21811 ) ;
#11983 = EDGE_CURVE ( 'NONE', #2593, #1809, #18854, .T. ) ;
#11984 = EDGE_CURVE ( 'NONE', #21686, #15874, #20393, .T. ) ;
#11985 = PLANE ( 'NONE',  #8468 ) ;
#11986 = CYLINDRICAL_SURFACE ( 'NONE', #21643, 3.175000000000149925 ) ;
#11987 = PRODUCT ( 'Support Ledge', 'Support Ledge', '', ( #11158 ) ) ;
#11988 = CARTESIAN_POINT ( 'NONE',  ( 142.2710730780391941, -3658.284631445515060, 2249.551220062097855 ) ) ;
#11989 = ORIENTED_EDGE ( 'NONE', *, *, #12962, .T. ) ;
#11990 = CARTESIAN_POINT ( 'NONE',  ( 136.8326944598556736, -3543.381058768859020, 2254.954196763766959 ) ) ;
#11991 = APPROVAL_PERSON_ORGANIZATION ( #11236, #19805, #2114 ) ;
#11992 = APPROVAL_PERSON_ORGANIZATION ( #20126, #17514, #20230 ) ;
#11993 = ORIENTED_EDGE ( 'NONE', *, *, #1416, .F. ) ;
#11994 = EDGE_CURVE ( 'NONE', #671, #204, #1038, .T. ) ;
#11995 = CARTESIAN_POINT ( 'NONE',  ( -12.70000000000005436, -3581.992340905245783, 2247.392000000001644 ) ) ;
#11996 = AXIS2_PLACEMENT_3D ( 'NONE', #20617, #16138, #17650 ) ;
#11997 = CARTESIAN_POINT ( 'NONE',  ( 116.8400000000000034, -3544.570000000000164, 2244.547199999999975 ) ) ;
#11998 = ORIENTED_EDGE ( 'NONE', *, *, #14233, .F. ) ;
#11999 = ORIENTED_EDGE ( 'NONE', *, *, #17102, .F. ) ;
#12000 = CARTESIAN_POINT ( 'NONE',  ( 4.762801830632181321, -3543.392327580375422, 2259.805458609068864 ) ) ;
#12001 = CARTESIAN_POINT ( 'NONE',  ( 88.90000000000000568, -3644.899999999999636, 2239.009999999999764 ) ) ;
#12002 = CARTESIAN_POINT ( 'NONE',  ( 146.1769999999999925, -3659.504999999999654, 2239.771999999999935 ) ) ;
#12003 = EDGE_LOOP ( 'NONE', ( #6083, #2988 ) ) ;
#12004 = CIRCLE ( 'NONE', #11621, 5.460999999999938126 ) ;
#12005 = CYLINDRICAL_SURFACE ( 'NONE', #22677, 5.460999999999938126 ) ;
#12006 = CARTESIAN_POINT ( 'NONE',  ( 139.6999999999999886, -3659.504999999999654, 2255.774000000000342 ) ) ;
#12007 = CARTESIAN_POINT ( 'NONE',  ( 139.6999999999999886, -3570.287499999999909, 2257.592639999999847 ) ) ;
#12008 = CARTESIAN_POINT ( 'NONE',  ( 18.34748010882359992, -3578.572769233774579, 2244.547227114076122 ) ) ;
#12009 = DIRECTION ( 'NONE',  ( -2.330758767204999802E-14, -1.000000000000000000, -1.206582004152999850E-12 ) ) ;
#12010 = EDGE_LOOP ( 'NONE', ( #13267, #18219, #7739, #6973 ) ) ;
#12011 = PRODUCT_CONTEXT ( 'NONE', #15162, 'mechanical' ) ;
#12012 = APPLICATION_CONTEXT ( 'configuration controlled 3d designs of mechanical parts and assemblies' ) ;
#12013 = EDGE_CURVE ( 'NONE', #12638, #9982, #16976, .T. ) ;
#12014 = ORIENTED_EDGE ( 'NONE', *, *, #22986, .T. ) ;
#12015 = CYLINDRICAL_SURFACE ( 'NONE', #4535, 3.175000000000149925 ) ;
#12016 = SECURITY_CLASSIFICATION ( '', '', #17657 ) ;
#12017 = PRODUCT_DEFINITION_FORMATION_WITH_SPECIFIED_SOURCE ( 'ANY', '', #3194, .NOT_KNOWN. ) ;
#12018 = CARTESIAN_POINT ( 'NONE',  ( 10.64300821491179683, -3581.461259321691614, 2248.549161679750796 ) ) ;
#12019 = LINE ( 'NONE', #4517, #9346 ) ;
#12020 = ORIENTED_EDGE ( 'NONE', *, *, #20569, .T. ) ;
#12021 = VECTOR ( 'NONE', #19285, 1000.000000000000000 ) ;
#12022 = ORIENTED_EDGE ( 'NONE', *, *, #628, .T. ) ;
#12023 = FACE_OUTER_BOUND ( 'NONE', #7838, .T. ) ;
#12024 = CIRCLE ( 'NONE', #13885, 3.606800000000000228 ) ;
#12025 = DIRECTION ( 'NONE',  ( 0.000000000000000000, 0.000000000000000000, -1.000000000000000000 ) ) ;
#12026 = CARTESIAN_POINT ( 'NONE',  ( 144.9086821617023588, -3661.856755788642204, 2245.123591690442936 ) ) ;
#12027 = DIRECTION ( 'NONE',  ( 0.000000000000000000, -1.000000000000000000, 0.000000000000000000 ) ) ;
#12028 = ADVANCED_FACE ( 'NONE', ( #4445 ), #12169, .T. ) ;
#12029 = CARTESIAN_POINT ( 'NONE',  ( 12.96232367102921579, -3662.340837267252027, 2249.194767252861766 ) ) ;
#12030 = CARTESIAN_POINT ( 'NONE',  ( 147.4569745407331141, -3543.701815209187771, 2260.256976450936236 ) ) ;
#12031 = ORIENTED_EDGE ( 'NONE', *, *, #6354, .F. ) ;
#12032 = CARTESIAN_POINT ( 'NONE',  ( 142.5447999999993272, -3579.946214629432234, 2256.063560000000962 ) ) ;
#12033 = DIRECTION ( 'NONE',  ( 1.000000000000000000, 0.000000000000000000, 0.000000000000000000 ) ) ;
#12034 = DIRECTION ( 'NONE',  ( 0.000000000000000000, 1.000000000000000000, 0.000000000000000000 ) ) ;
#12035 = CARTESIAN_POINT ( 'NONE',  ( 15.05256792404641075, -3657.905201311359178, 2249.153143157146587 ) ) ;
#12036 = DIRECTION ( 'NONE',  ( 0.000000000000000000, -1.000000000000000000, 0.000000000000000000 ) ) ;
#12037 = ORIENTED_EDGE ( 'NONE', *, *, #3248, .T. ) ;
#12038 = AXIS2_PLACEMENT_3D ( 'NONE', #15157, #7785, #21849 ) ;
#12039 = ORIENTED_EDGE ( 'NONE', *, *, #15026, .F. ) ;
#12040 = VECTOR ( 'NONE', #15375, 1000.000000000000000 ) ;
#12041 = ORIENTED_EDGE ( 'NONE', *, *, #16011, .F. ) ;
#12042 = ORIENTED_EDGE ( 'NONE', *, *, #14820, .T. ) ;
#12043 = FACE_OUTER_BOUND ( 'NONE', #23079, .T. ) ;
#12044 = CARTESIAN_POINT ( 'NONE',  ( 15.24000000000000021, -3695.699999999999818, 2255.774000000000342 ) ) ;
#12045 = DIRECTION ( 'NONE',  ( 0.000000000000000000, -1.000000000000000000, 0.000000000000000000 ) ) ;
#12046 = CARTESIAN_POINT ( 'NONE',  ( 11.34365660143000021, -3581.844255679000071, 2239.391000000000076 ) ) ;
#12047 = CARTESIAN_POINT ( 'NONE',  ( 15.53593155406000115, -3659.229969269999856, 2257.960590233999937 ) ) ;
#12048 = DIRECTION ( 'NONE',  ( 0.000000000000000000, 0.000000000000000000, 1.000000000000000000 ) ) ;
#12049 = CIRCLE ( 'NONE', #3876, 1.523999999999858801 ) ;
#12050 = CARTESIAN_POINT ( 'NONE',  ( -6.349999999999880629, -3578.860000000000127, 2252.472000000000207 ) ) ;
#12051 = ORIENTED_EDGE ( 'NONE', *, *, #21056, .F. ) ;
#12052 = CIRCLE ( 'NONE', #3823, 0.3809999999999647002 ) ;
#12053 = DIRECTION ( 'NONE',  ( -2.903809793931999834E-13, 4.457650181899999573E-12, 1.000000000000000000 ) ) ;
#12054 = CIRCLE ( 'NONE', #6815, 3.606799999998994366 ) ;
#12055 = FACE_OUTER_BOUND ( 'NONE', #77, .T. ) ;
#12056 = EDGE_LOOP ( 'NONE', ( #21294, #7472, #13803, #22740, #5292, #2951 ) ) ;
#12057 = LINE ( 'NONE', #19211, #4683 ) ;
#12058 = CARTESIAN_POINT ( 'NONE',  ( 10.11254281055728299, -3658.322299598116388, 2249.580929887502862 ) ) ;
#12059 = ORIENTED_EDGE ( 'NONE', *, *, #18998, .F. ) ;
#12060 = ORIENTED_EDGE ( 'NONE', *, *, #6221, .T. ) ;
#12061 = DIRECTION ( 'NONE',  ( -1.000000000000000000, 0.000000000000000000, 0.000000000000000000 ) ) ;
#12062 = VECTOR ( 'NONE', #18016, 1000.000000000000000 ) ;
#12063 = EDGE_LOOP ( 'NONE', ( #17553, #18710, #4886, #18514, #16213 ) ) ;
#12064 = DIRECTION ( 'NONE',  ( -0.000000000000000000, -1.000000000000000000, -0.000000000000000000 ) ) ;
#12065 = APPROVAL_STATUS ( 'not_yet_approved' ) ;
#12066 = AXIS2_PLACEMENT_3D ( 'NONE', #20948, #10044, #17538 ) ;
#12067 = ORIENTED_EDGE ( 'NONE', *, *, #20113, .F. ) ;
#12068 = CARTESIAN_POINT ( 'NONE',  ( 132.0226525136210967, -3695.032413813642052, 2260.455666005582316 ) ) ;
#12069 = APPROVAL_ROLE ( '' ) ;
#12070 = APPROVAL ( #6263, 'UNSPECIFIED' ) ;
#12071 = AXIS2_PLACEMENT_3D ( 'NONE', #5132, #22450, #8177 ) ;
#12072 = CARTESIAN_POINT ( 'NONE',  ( 21.79320000000099711, -3619.500000000000000, 2259.837999999999738 ) ) ;
#12073 = CARTESIAN_POINT ( 'NONE',  ( 14.48688036290512038, -3581.708692406665250, 2247.466127284272716 ) ) ;
#12074 = CARTESIAN_POINT ( 'NONE',  ( 134.2236363864670636, -3657.869847840709099, 2245.675467034049689 ) ) ;
#12075 = EDGE_CURVE ( 'NONE', #9663, #16380, #13588, .T. ) ;
#12076 = EDGE_CURVE ( 'NONE', #4616, #6734, #18731, .T. ) ;
#12077 = DIRECTION ( 'NONE',  ( 0.000000000000000000, 0.000000000000000000, -1.000000000000000000 ) ) ;
#12078 = VERTEX_POINT ( 'NONE', #4673 ) ;
#12079 = DIRECTION ( 'NONE',  ( 0.000000000000000000, 0.000000000000000000, 1.000000000000000000 ) ) ;
#12080 = ADVANCED_FACE ( 'NONE', ( #15233 ), #11824, .T. ) ;
#12081 = ORIENTED_EDGE ( 'NONE', *, *, #21106, .T. ) ;
#12082 = CARTESIAN_POINT ( 'NONE',  ( 14.27729191008000065, -3577.121900051000011, 2257.704292951999832 ) ) ;
#12083 = VERTEX_POINT ( 'NONE', #16861 ) ;
#12084 = DIRECTION ( 'NONE',  ( 0.000000000000000000, 0.000000000000000000, 1.000000000000000000 ) ) ;
#12085 = VECTOR ( 'NONE', #10945, 1000.000000000000000 ) ;
#12086 = TOROIDAL_SURFACE ( 'NONE', #14344, 4.114799999999999791, 1.270000000000000018 ) ;
#12087 = CARTESIAN_POINT ( 'NONE',  ( 15.54479999999999862, -3639.502500000000055, 2263.571799999999712 ) ) ;
#12088 = ORIENTED_EDGE ( 'NONE', *, *, #17741, .F. ) ;
#12089 = EDGE_CURVE ( 'NONE', #18860, #17851, #10289, .T. ) ;
#12090 = CARTESIAN_POINT ( 'NONE',  ( 20.34169023495000062, -3544.202533098000458, 2260.545675974999995 ) ) ;
#12091 = CARTESIAN_POINT ( 'NONE',  ( 134.0147555151665699, -3660.087502428663811, 2244.547653756476848 ) ) ;
#12092 = ORIENTED_EDGE ( 'NONE', *, *, #20383, .T. ) ;
#12093 = FACE_BOUND ( 'NONE', #8123, .T. ) ;
#12094 = CARTESIAN_POINT ( 'NONE',  ( 15.54478274856999853, -3659.614687031725680, 2250.189939678317842 ) ) ;
#12095 = DIRECTION ( 'NONE',  ( 1.000000000000000000, 0.000000000000000000, 0.000000000000000000 ) ) ;
#12096 = EDGE_CURVE ( 'NONE', #4791, #3607, #11583, .T. ) ;
#12097 = DIRECTION ( 'NONE',  ( 1.000000000000000000, 0.000000000000000000, 0.000000000000000000 ) ) ;
#12098 = VECTOR ( 'NONE', #18502, 1000.000000000000000 ) ;
#12099 = CALENDAR_DATE ( 2026, 26, 10 ) ;
#12100 = EDGE_LOOP ( 'NONE', ( #7767, #6319 ) ) ;
#12101 = AXIS2_PLACEMENT_3D ( 'NONE', #10750, #4568, #17895 ) ;
#12102 = DIRECTION ( 'NONE',  ( -1.000000000000000000, 0.000000000000000000, 0.000000000000000000 ) ) ;
#12103 = CARTESIAN_POINT ( 'NONE',  ( 136.8552000000009912, -3579.494999999999891, 2272.030000000000200 ) ) ;
#12104 = DIRECTION ( 'NONE',  ( -1.000000000000000000, 0.000000000000000000, 0.000000000000000000 ) ) ;
#12105 = AXIS2_PLACEMENT_3D ( 'NONE', #22279, #22513, #8127 ) ;
#12106 = CARTESIAN_POINT ( 'NONE',  ( 141.7270126280175475, -3657.507999012949767, 2248.476214850042652 ) ) ;
#12107 = ORIENTED_EDGE ( 'NONE', *, *, #7962, .F. ) ;
#12108 = EDGE_CURVE ( 'NONE', #13681, #14824, #8663, .T. ) ;
#12109 = EDGE_CURVE ( 'NONE', #5628, #21067, #7140, .T. ) ;
#12110 = VERTEX_POINT ( 'NONE', #19559 ) ;
#12111 = VERTEX_POINT ( 'NONE', #13939 ) ;
#12112 = CIRCLE ( 'NONE', #19598, 2.844799999999009010 ) ;
#12113 = CARTESIAN_POINT ( 'NONE',  ( 12.70000000003999929, -3662.637340904999746, 2239.009999999999764 ) ) ;
#12114 = ORIENTED_EDGE ( 'NONE', *, *, #3269, .F. ) ;
#12115 = VERTEX_POINT ( 'NONE', #21086 ) ;
#12116 = CYLINDRICAL_SURFACE ( 'NONE', #2294, 0.7619999999999230722 ) ;
#12117 = FACE_OUTER_BOUND ( 'NONE', #15468, .T. ) ;
#12118 = CARTESIAN_POINT ( 'NONE',  ( 15.24000000000000021, -3580.776127254000130, 2255.774000000000342 ) ) ;
#12119 = ORIENTED_EDGE ( 'NONE', *, *, #15662, .T. ) ;
#12120 = FACE_OUTER_BOUND ( 'NONE', #15999, .T. ) ;
#12121 = DIRECTION ( 'NONE',  ( 0.000000000000000000, 1.000000000000000000, 0.000000000000000000 ) ) ;
#12122 = DIRECTION ( 'NONE',  ( -2.336881798971000105E-14, 0.000000000000000000, -1.000000000000000000 ) ) ;
#12123 = DIRECTION ( 'NONE',  ( -1.224646799141892071E-16, -1.000000000000000000, 2.336881798971000421E-14 ) ) ;
#12124 = ORIENTED_EDGE ( 'NONE', *, *, #12607, .F. ) ;
#12125 = DATE_AND_TIME ( #4982, #7901 ) ;
#12126 = ORIENTED_EDGE ( 'NONE', *, *, #10277, .T. ) ;
#12127 = CARTESIAN_POINT ( 'NONE',  ( 12.69999999999999929, -3585.210000000000036, 2268.705139999999574 ) ) ;
#12128 = EDGE_LOOP ( 'NONE', ( #13198, #9052, #14482, #10838 ) ) ;
#12129 = TOROIDAL_SURFACE ( 'NONE', #17349, 4.114799999999999791, 1.270000000000000018 ) ;
#12130 = CARTESIAN_POINT ( 'NONE',  ( 10.58260127282864538, -3581.394912766336802, 2248.683245035067102 ) ) ;
#12131 = EDGE_LOOP ( 'NONE', ( #14346, #21823 ) ) ;
#12132 = CARTESIAN_POINT ( 'NONE',  ( 0.7620000000000000107, -3543.299999999999727, 2238.248000000000047 ) ) ;
#12133 = AXIS2_PLACEMENT_3D ( 'NONE', #13910, #1363, #7009 ) ;
#12134 = B_SPLINE_CURVE_WITH_KNOTS ( 'NONE', 3,
 ( #22846, #3054, #13846, #11964, #19114, #14079, #15608, #3291, #19234, #15, #17697, #19580, #13732, #14199, #17466, #22738, #15950, #5179, #8685, #12319, #7056, #6819, #10203, #17340 ),
 .UNSPECIFIED., .F., .F.,
 ( 4, 2, 2, 1, 1, 1, 2, 2, 2, 2, 1, 2, 2, 4 ),
 ( 0.000000000000000000, 0.1250000000064511452, 0.1875000000096775921, 0.2187500000117214016, 0.2343750000127438893, 0.2421875000132545364, 0.2460937500135104705, 0.2500000000137663769, 0.3750000000113288823, 0.4375000000103546061, 0.4687500000103158038, 0.4843750000103104192, 0.5000000000103050901, 1.000000000000000000 ),
 .UNSPECIFIED. ) ;
#12135 = VERTEX_POINT ( 'NONE', #3495 ) ;
#12136 = ORIENTED_EDGE ( 'NONE', *, *, #14019, .T. ) ;
#12137 = DIRECTION ( 'NONE',  ( 0.000000000000000000, 0.000000000000000000, -1.000000000000000000 ) ) ;
#12138 = DIRECTION ( 'NONE',  ( 2.336881798971000105E-14, 2.336881798971000105E-14, 1.000000000000000000 ) ) ;
#12139 = LINE ( 'NONE', #3234, #12968 ) ;
#12140 = CARTESIAN_POINT ( 'NONE',  ( 11.42511155983525839, -3662.048141298665541, 2249.501989319668610 ) ) ;
#12141 = EDGE_CURVE ( 'NONE', #16613, #11557, #13278, .T. ) ;
#12142 = ADVANCED_FACE ( 'NONE', ( #15809 ), #14250, .T. ) ;
#12143 = CARTESIAN_POINT ( 'NONE',  ( 142.0316867971391446, -3658.158799999964231, 2239.391000000000076 ) ) ;
#12144 = ORIENTED_EDGE ( 'NONE', *, *, #11146, .T. ) ;
#12145 = EDGE_CURVE ( 'NONE', #12156, #13472, #17794, .T. ) ;
#12146 = B_SPLINE_CURVE_WITH_KNOTS ( 'NONE', 3,
 ( #16034, #12399, #5499, #7247 ),
 .UNSPECIFIED., .F., .F.,
 ( 4, 4 ),
 ( 0.000000000000000000, 1.000000000000000000 ),
 .UNSPECIFIED. ) ;
#12147 = DIRECTION ( 'NONE',  ( 0.000000000000000000, 0.000000000000000000, 1.000000000000000000 ) ) ;
#12148 = VECTOR ( 'NONE', #20469, 1000.000000000000000 ) ;
#12149 = CIRCLE ( 'NONE', #14784, 3.606799999999993567 ) ;
#12150 = CARTESIAN_POINT ( 'NONE',  ( -6.349999999999999645, -3660.140000000000327, 2243.785200000000259 ) ) ;
#12151 = VECTOR ( 'NONE', #17736, 1000.000000000000000 ) ;
#12152 = CARTESIAN_POINT ( 'NONE',  ( 15.26350286127714284, -3658.268776985493332, 2249.537495782451060 ) ) ;
#12153 = CARTESIAN_POINT ( 'NONE',  ( 40.94480000000000075, -3644.899999999999636, 2261.869999999999891 ) ) ;
#12154 = EDGE_LOOP ( 'NONE', ( #687, #8625, #18730, #13321 ) ) ;
#12155 = EDGE_CURVE ( 'NONE', #16634, #17242, #10533, .T. ) ;
#12156 = VERTEX_POINT ( 'NONE', #14288 ) ;
#12157 = FACE_OUTER_BOUND ( 'NONE', #9287, .T. ) ;
#12158 = EDGE_LOOP ( 'NONE', ( #14662, #6505, #20556, #15520 ) ) ;
#12159 = DIRECTION ( 'NONE',  ( -1.000000000000000000, 0.000000000000000000, 0.000000000000000000 ) ) ;
#12160 = SECURITY_CLASSIFICATION_LEVEL ( 'unclassified' ) ;
#12161 = EDGE_CURVE ( 'NONE', #4345, #5555, #5386, .T. ) ;
#12162 = FACE_OUTER_BOUND ( 'NONE', #4277, .T. ) ;
#12163 = EDGE_CURVE ( 'NONE', #5531, #5311, #14056, .T. ) ;
#12164 = CARTESIAN_POINT ( 'NONE',  ( 12.42449270472999956, -3656.669101290000071, 2257.594923725999706 ) ) ;
#12165 = DIRECTION ( 'NONE',  ( 0.000000000000000000, 0.000000000000000000, 1.000000000000000000 ) ) ;
#12166 = CIRCLE ( 'NONE', #1669, 1.904999999999823501 ) ;
#12167 = VECTOR ( 'NONE', #11410, 1000.000000000000000 ) ;
#12168 = DIRECTION ( 'NONE',  ( 0.000000000000000000, 0.000000000000000000, -1.000000000000000000 ) ) ;
#12169 = TOROIDAL_SURFACE ( 'NONE', #19282, 3.606799999998999695, 0.7620000000000000107 ) ;
#12170 = CARTESIAN_POINT ( 'NONE',  ( 15.03168679716000078, -3578.148799999999937, 2242.820000000000164 ) ) ;
#12171 = AXIS2_PLACEMENT_3D ( 'NONE', #21120, #10212, #6829 ) ;
#12172 = DIRECTION ( 'NONE',  ( 2.330758767201999921E-14, 1.000000000000000000, 0.000000000000000000 ) ) ;
#12173 = VERTEX_POINT ( 'NONE', #8554 ) ;
#12174 =( BOUNDED_CURVE ( )  B_SPLINE_CURVE ( 3, ( #18758, #22156, #6131, #13256 ),
 .UNSPECIFIED., .F., .T. ) 
 B_SPLINE_CURVE_WITH_KNOTS ( ( 4, 4 ),
 ( 1.570796326809868804, 3.141592653589801110 ),
 .UNSPECIFIED. ) 
 CURVE ( )  GEOMETRIC_REPRESENTATION_ITEM ( )  RATIONAL_B_SPLINE_CURVE ( ( 1.000000000000000000, 0.8047378541278922270, 0.8047378541278922270, 1.000000000000000000 ) ) 
 REPRESENTATION_ITEM ( '' )  );
#12175 = CARTESIAN_POINT ( 'NONE',  ( -5.588000000000000078, -3694.938000000000102, 2228.849999999999909 ) ) ;
#12176 = LINE ( 'NONE', #2211, #5453 ) ;
#12177 = VERTEX_POINT ( 'NONE', #12410 ) ;
#12178 = CARTESIAN_POINT ( 'NONE',  ( 8.088613972650000150, -3576.119152860999748, 2246.630000000000109 ) ) ;
#12179 = CARTESIAN_POINT ( 'NONE',  ( 10.06210023420644184, -3658.439931164731206, 2249.672963766948669 ) ) ;
#12180 = VERTEX_POINT ( 'NONE', #19674 ) ;
#12181 = CARTESIAN_POINT ( 'NONE',  ( 132.0879339926999876, -3694.758336080999925, 2260.533847755999886 ) ) ;
#12182 = AXIS2_PLACEMENT_3D ( 'NONE', #13463, #3030, #1267 ) ;
#12183 = ORIENTED_EDGE ( 'NONE', *, *, #14591, .F. ) ;
#12184 = PLANE ( 'NONE',  #20083 ) ;
#12185 = COORDINATED_UNIVERSAL_TIME_OFFSET ( 0, 0, .AHEAD. ) ;
#12186 = CIRCLE ( 'NONE', #14065, 1.269999999999882334 ) ;
#12187 = LINE ( 'NONE', #19103, #21092 ) ;
#12188 = ORIENTED_EDGE ( 'NONE', *, *, #23160, .F. ) ;
#12189 = CARTESIAN_POINT ( 'NONE',  ( 131.9181769293102207, -3695.361398937724971, 2260.194562468291679 ) ) ;
#12190 = CIRCLE ( 'NONE', #15185, 5.080000000000000071 ) ;
#12191 = PRODUCT_CONTEXT ( 'NONE', #22030, 'mechanical' ) ;
#12192 = CARTESIAN_POINT ( 'NONE',  ( 54.40679999999999694, -3670.300000000000182, 2239.771999999999935 ) ) ;
#12193 = CARTESIAN_POINT ( 'NONE',  ( 12.69999999999999929, -3590.289999999999964, 2268.705139999999574 ) ) ;
#12194 = CARTESIAN_POINT ( 'NONE',  ( 133.9990844033331427, -3659.101433724999879, 2244.742833232057365 ) ) ;
#12195 = AXIS2_PLACEMENT_3D ( 'NONE', #6421, #16833, #20361 ) ;
#12196 = CARTESIAN_POINT ( 'NONE',  ( 139.7000000002931301, -3656.372659094888149, 2239.009999999999764 ) ) ;
#12197 = VERTEX_POINT ( 'NONE', #19329 ) ;
#12198 = VECTOR ( 'NONE', #20143, 1000.000000000000000 ) ;
#12199 = DIRECTION ( 'NONE',  ( 0.000000000000000000, 0.000000000000000000, 1.000000000000000000 ) ) ;
#12200 = CARTESIAN_POINT ( 'NONE',  ( 127.0000000000000000, -3568.700000000000273, 2259.837999999999738 ) ) ;
#12201 = ORIENTED_EDGE ( 'NONE', *, *, #13288, .T. ) ;
#12202 = FACE_OUTER_BOUND ( 'NONE', #3895, .T. ) ;
#12203 = CIRCLE ( 'NONE', #10721, 3.606800000000000228 ) ;
#12204 = APPROVAL ( #11597, 'UNSPECIFIED' ) ;
#12205 = DIRECTION ( 'NONE',  ( 1.000000000000000000, 0.000000000000000000, 0.000000000000000000 ) ) ;
#12206 = CIRCLE ( 'NONE', #15204, 0.7619999999999294005 ) ;
#12207 = VERTEX_POINT ( 'NONE', #3266 ) ;
#12208 = ORIENTED_EDGE ( 'NONE', *, *, #19906, .F. ) ;
#12209 = CARTESIAN_POINT ( 'NONE',  ( 127.0000000000000000, -3619.500000000000000, 2260.600000000000364 ) ) ;
#12210 = DIRECTION ( 'NONE',  ( -2.324635735433000053E-14, 2.336881798971000105E-14, -1.000000000000000000 ) ) ;
#12211 = VERTEX_POINT ( 'NONE', #21211 ) ;
#12212 = CARTESIAN_POINT ( 'NONE',  ( 10.16000000000000014, -3658.223872745999870, 2255.774000000000342 ) ) ;
#12213 = CARTESIAN_POINT ( 'NONE',  ( 15.47556979461559123, -3660.128696051647694, 2250.236801090939025 ) ) ;
#12214 = EDGE_CURVE ( 'NONE', #2445, #11162, #11790, .T. ) ;
#12215 = DIRECTION ( 'NONE',  ( 1.000000000000000000, 5.432398939370942693E-28, -2.324635735433000053E-14 ) ) ;
#12216 = B_SPLINE_CURVE_WITH_KNOTS ( 'NONE', 3,
 ( #8498, #3092, #15643, #6979 ),
 .UNSPECIFIED., .F., .F.,
 ( 4, 4 ),
 ( 0.000000000000000000, 1.000000000000000000 ),
 .UNSPECIFIED. ) ;
#12217 = DIRECTION ( 'NONE',  ( 0.000000000000000000, 0.000000000000000000, -1.000000000000000000 ) ) ;
#12218 = PERSON_AND_ORGANIZATION ( #5446, #1895 ) ;
#12219 = EDGE_CURVE ( 'NONE', #15231, #11877, #3379, .T. ) ;
#12220 = TOROIDAL_SURFACE ( 'NONE', #5497, 5.080000000000000071, 0.3810000000000000053 ) ;
#12221 = CARTESIAN_POINT ( 'NONE',  ( 61.26424768829000556, -3543.299999999999727, 2279.065800000000309 ) ) ;
#12222 = DIRECTION ( 'NONE',  ( 1.000000000000000000, 0.000000000000000000, 0.000000000000000000 ) ) ;
#12223 = CARTESIAN_POINT ( 'NONE',  ( 18.37619926079141308, -3580.159608052614658, 2244.861392947899731 ) ) ;
#12224 = CIRCLE ( 'NONE', #3655, 5.587999999999926359 ) ;
#12225 = CIRCLE ( 'NONE', #21585, 5.460999999999938126 ) ;
#12226 = CARTESIAN_POINT ( 'NONE',  ( 141.8375137957061156, -3657.627758956946764, 2248.726790701012305 ) ) ;
#12227 = AXIS2_PLACEMENT_3D ( 'NONE', #17640, #19177, #6883 ) ;
#12228 = ORIENTED_EDGE ( 'NONE', *, *, #11669, .T. ) ;
#12229 = DIRECTION ( 'NONE',  ( 0.000000000000000000, 0.000000000000000000, 1.000000000000000000 ) ) ;
#12230 = ORIENTED_EDGE ( 'NONE', *, *, #20896, .F. ) ;
#12231 = EDGE_LOOP ( 'NONE', ( #12917, #10556, #2995, #11969 ) ) ;
#12232 = ORIENTED_EDGE ( 'NONE', *, *, #20460, .T. ) ;
#12233 = AXIS2_PLACEMENT_3D ( 'NONE', #17112, #4578, #4241 ) ;
#12234 = AXIS2_PLACEMENT_3D ( 'NONE', #1930, #16223, #4036 ) ;
#12235 = DIRECTION ( 'NONE',  ( 1.000000000000000000, 0.000000000000000000, -1.224646799147353207E-16 ) ) ;
#12236 = ORIENTED_EDGE ( 'NONE', *, *, #22315, .F. ) ;
#12237 = ORIENTED_EDGE ( 'NONE', *, *, #18401, .F. ) ;
#12238 = DIRECTION ( 'NONE',  ( 0.000000000000000000, 1.000000000000000000, 0.000000000000000000 ) ) ;
#12239 = PERSON_AND_ORGANIZATION_ROLE ( 'classification_officer' ) ;
#12240 = DIRECTION ( 'NONE',  ( 0.000000000000000000, -1.000000000000000000, 0.000000000000000000 ) ) ;
#12241 = CIRCLE ( 'NONE', #17846, 2.844800000000091700 ) ;
#12242 = DIRECTION ( 'NONE',  ( 0.000000000000000000, 0.000000000000000000, -1.000000000000000000 ) ) ;
#12243 = ORIENTED_EDGE ( 'NONE', *, *, #22253, .T. ) ;
#12244 = DIRECTION ( 'NONE',  ( 0.000000000000000000, 0.000000000000000000, 1.000000000000000000 ) ) ;
#12245 = EDGE_CURVE ( 'NONE', #20246, #14593, #1299, .T. ) ;
#12246 = AXIS2_PLACEMENT_3D ( 'NONE', #19766, #2292, #14493 ) ;
#12247 = DIRECTION ( 'NONE',  ( 0.000000000000000000, 0.000000000000000000, 1.000000000000000000 ) ) ;
#12248 = FACE_OUTER_BOUND ( 'NONE', #11531, .T. ) ;
#12249 = CARTESIAN_POINT ( 'NONE',  ( 142.2400000000000091, -3660.786127253999894, 2255.774000000000342 ) ) ;
#12250 = EDGE_CURVE ( 'NONE', #21408, #8087, #21161, .T. ) ;
#12251 = ORIENTED_EDGE ( 'NONE', *, *, #18022, .T. ) ;
#12252 = CALENDAR_DATE ( 2026, 26, 10 ) ;
#12253 = EDGE_CURVE ( 'NONE', #2858, #257, #6187, .T. ) ;
#12254 = ORIENTED_EDGE ( 'NONE', *, *, #22504, .F. ) ;
#12255 = LINE ( 'NONE', #15769, #8293 ) ;
#12256 = CARTESIAN_POINT ( 'NONE',  ( 10.05562585061285219, -3580.543848469380919, 2249.684969000971705 ) ) ;
#12257 = VECTOR ( 'NONE', #6236, 1000.000000000000000 ) ;
#12258 = ORIENTED_EDGE ( 'NONE', *, *, #11274, .T. ) ;
#12259 = DIRECTION ( 'NONE',  ( -1.000000000000000000, 0.000000000000000000, 0.000000000000000000 ) ) ;
#12260 = EDGE_LOOP ( 'NONE', ( #4528, #14465, #21759, #6067 ) ) ;
#12261 = CARTESIAN_POINT ( 'NONE',  ( 12.69999999999999929, -3589.528000000000247, 2268.705139999999574 ) ) ;
#12262 = AXIS2_PLACEMENT_3D ( 'NONE', #7133, #1971, #19548 ) ;
#12263 = AXIS2_PLACEMENT_3D ( 'NONE', #9846, #18996, #10075 ) ;
#12264 = ADVANCED_FACE ( 'NONE', ( #5263 ), #17911, .F. ) ;
#12265 = DIRECTION ( 'NONE',  ( 0.000000000000000000, -1.000000000000000000, 0.000000000000000000 ) ) ;
#12266 = CARTESIAN_POINT ( 'NONE',  ( 123.3932000000010021, -3670.300000000000182, 2239.771999999999935 ) ) ;
#12267 = CARTESIAN_POINT ( 'NONE',  ( 11.02929805643817396, -3661.807647569477467, 2249.696627142566285 ) ) ;
#12268 = LINE ( 'NONE', #3351, #16674 ) ;
#12269 = VERTEX_POINT ( 'NONE', #4911 ) ;
#12270 = DIRECTION ( 'NONE',  ( -2.334777064352623371E-14, -1.000000000000000000, 0.000000000000000000 ) ) ;
#12271 = CARTESIAN_POINT ( 'NONE',  ( 12.70000000003999929, -3582.187399999999798, 2239.391000000000076 ) ) ;
#12272 = AXIS2_PLACEMENT_3D ( 'NONE', #19021, #4486, #9344 ) ;
#12273 = PLANE ( 'NONE',  #10441 ) ;
#12274 = CARTESIAN_POINT ( 'NONE',  ( 14.66806072689505314, -3657.450396280145469, 2248.320112768498348 ) ) ;
#12275 = FACE_OUTER_BOUND ( 'NONE', #19162, .T. ) ;
#12276 = ORIENTED_EDGE ( 'NONE', *, *, #18326, .T. ) ;
#12277 = DIRECTION ( 'NONE',  ( 0.000000000000000000, 1.000000000000000000, 1.224646799147353207E-16 ) ) ;
#12278 = ORIENTED_EDGE ( 'NONE', *, *, #10260, .T. ) ;
#12279 = CIRCLE ( 'NONE', #14526, 0.3809999999999647002 ) ;
#12280 = EDGE_CURVE ( 'NONE', #7536, #22551, #12057, .T. ) ;
#12281 = CARTESIAN_POINT ( 'NONE',  ( -12.31900000000000084, -3660.140000000000327, 2247.392000000000280 ) ) ;
#12282 = LINE ( 'NONE', #10516, #18253 ) ;
#12283 = PERSON_AND_ORGANIZATION_ROLE ( 'classification_officer' ) ;
#12284 = EDGE_CURVE ( 'NONE', #5265, #8260, #10298, .T. ) ;
#12285 = FACE_OUTER_BOUND ( 'NONE', #5586, .T. ) ;
#12286 = ADVANCED_FACE ( 'NONE', ( #4189 ), #18368, .T. ) ;
#12287 = DIRECTION ( 'NONE',  ( -1.000000000000000000, 0.000000000000000000, 0.000000000000000000 ) ) ;
#12288 = DIRECTION ( 'NONE',  ( 0.000000000000000000, 0.000000000000000000, 1.000000000000000000 ) ) ;
#12289 = DIRECTION ( 'NONE',  ( 0.000000000000000000, 0.000000000000000000, -1.000000000000000000 ) ) ;
#12290 = LINE ( 'NONE', #21316, #21476 ) ;
#12291 = AXIS2_PLACEMENT_3D ( 'NONE', #2372, #2590, #15135 ) ;
#12292 = FACE_OUTER_BOUND ( 'NONE', #18265, .T. ) ;
#12293 = EDGE_CURVE ( 'NONE', #5417, #8367, #17785, .T. ) ;
#12294 = ORIENTED_EDGE ( 'NONE', *, *, #3343, .F. ) ;
#12295 = FACE_OUTER_BOUND ( 'NONE', #784, .T. ) ;
#12296 = CARTESIAN_POINT ( 'NONE',  ( 12.69999999999999929, -3639.502500000000055, 2290.622800000000097 ) ) ;
#12297 = ORIENTED_EDGE ( 'NONE', *, *, #22463, .F. ) ;
#12298 = DIRECTION ( 'NONE',  ( 0.000000000000000000, 0.000000000000000000, 1.000000000000000000 ) ) ;
#12299 = EDGE_CURVE ( 'NONE', #16784, #2492, #11047, .T. ) ;
#12300 = ADVANCED_FACE ( 'NONE', ( #448 ), #9130, .F. ) ;
#12301 = ORIENTED_EDGE ( 'NONE', *, *, #5391, .F. ) ;
#12302 = CARTESIAN_POINT ( 'NONE',  ( 3.810000000000000053, -3695.699999999999818, 2228.849999999999909 ) ) ;
#12303 = EDGE_LOOP ( 'NONE', ( #15618, #13468 ) ) ;
#12304 = VERTEX_POINT ( 'NONE', #12873 ) ;
#12305 = CARTESIAN_POINT ( 'NONE',  ( 12.70000000000085194, -3602.342301254449922, 2279.817638608976267 ) ) ;
#12306 = APPROVAL_DATE_TIME ( #5166, #16097 ) ;
#12307 = CYLINDRICAL_SURFACE ( 'NONE', #6460, 1.269999999999900320 ) ;
#12308 = ORIENTED_EDGE ( 'NONE', *, *, #12284, .T. ) ;
#12309 = CIRCLE ( 'NONE', #19046, 5.080000000000000959 ) ;
#12310 = DIRECTION ( 'NONE',  ( 0.000000000000000000, 0.000000000000000000, -1.000000000000000000 ) ) ;
#12311 = CALENDAR_DATE ( 2026, 26, 10 ) ;
#12312 = ADVANCED_FACE ( 'NONE', ( #336 ), #7683, .T. ) ;
#12313 = CARTESIAN_POINT ( 'NONE',  ( 145.4150000000009868, -3579.494999999999891, 2239.771999999999935 ) ) ;
#12314 = CARTESIAN_POINT ( 'NONE',  ( 15.06015184098700743, -3581.085670991564712, 2249.167371890592221 ) ) ;
#12315 = CARTESIAN_POINT ( 'NONE',  ( 3.048000000000000043, -3544.061999999999898, 2229.612000000000080 ) ) ;
#12316 = DIRECTION ( 'NONE',  ( 0.000000000000000000, 0.000000000000000000, -1.000000000000000000 ) ) ;
#12317 = DIRECTION ( 'NONE',  ( 0.000000000000000000, 0.000000000000000000, 1.000000000000000000 ) ) ;
#12318 = VERTEX_POINT ( 'NONE', #21890 ) ;
#12319 = CARTESIAN_POINT ( 'NONE',  ( 15.38815085373434322, -3695.327183877504467, 2255.402917874296691 ) ) ;
#12320 = CARTESIAN_POINT ( 'NONE',  ( 97.99320000000000164, -3619.500000000000000, 2259.837999999999738 ) ) ;
#12321 = ORIENTED_EDGE ( 'NONE', *, *, #5855, .F. ) ;
#12322 = VECTOR ( 'NONE', #199, 1000.000000000000000 ) ;
#12323 = DIRECTION ( 'NONE',  ( -0.7071067811865969777, 0.000000000000000000, -0.7071067811864980568 ) ) ;
#12324 = ADVANCED_FACE ( 'NONE', ( #12990 ), #12755, .F. ) ;
#12325 = DIRECTION ( 'NONE',  ( 0.000000000000000000, 0.000000000000000000, 1.000000000000000000 ) ) ;
#12326 = ORIENTED_EDGE ( 'NONE', *, *, #22514, .T. ) ;
#12327 = DIRECTION ( 'NONE',  ( 0.000000000000000000, -1.000000000000000000, 0.000000000000000000 ) ) ;
#12328 = ORIENTED_EDGE ( 'NONE', *, *, #12145, .F. ) ;
#12329 = CARTESIAN_POINT ( 'NONE',  ( 139.6999999999999886, -3579.494999999999891, 2239.771999999999935 ) ) ;
#12330 = CYLINDRICAL_SURFACE ( 'NONE', #13328, 11.11249999999985860 ) ;
#12331 = DIRECTION ( 'NONE',  ( -1.000000000000000000, 0.000000000000000000, 0.000000000000000000 ) ) ;
#12332 = APPLICATION_PROTOCOL_DEFINITION ( 'international standard', 'automotive_design', 2000, #2877 ) ;
#12333 = AXIS2_PLACEMENT_3D ( 'NONE', #10490, #17632, #1464 ) ;
#12334 = FACE_OUTER_BOUND ( 'NONE', #6639, .T. ) ;
#12335 = LINE ( 'NONE', #17842, #16910 ) ;
#12336 = PLANE ( 'NONE',  #13781 ) ;
#12337 = AXIS2_PLACEMENT_3D ( 'NONE', #13053, #22172, #9529 ) ;
#12338 = APPLIED_DATE_AND_TIME_ASSIGNMENT ( #12700, #18738, ( #2304 ) ) ;
#12339 = FACE_OUTER_BOUND ( 'NONE', #6496, .T. ) ;
#12340 = B_SPLINE_CURVE_WITH_KNOTS ( 'NONE', 3,
 ( #18941, #8278, #15200, #22439 ),
 .UNSPECIFIED., .F., .F.,
 ( 4, 4 ),
 ( 0.000000000000000000, 1.000000000000000000 ),
 .UNSPECIFIED. ) ;
#12341 = ORIENTED_EDGE ( 'NONE', *, *, #3799, .T. ) ;
#12342 = CARTESIAN_POINT ( 'NONE',  ( 0.7620000000000000107, -3544.061999999999898, 2275.763800000000174 ) ) ;
#12343 = ORIENTED_EDGE ( 'NONE', *, *, #7414, .T. ) ;
#12344 = ORIENTED_EDGE ( 'NONE', *, *, #1712, .F. ) ;
#12345 = EDGE_LOOP ( 'NONE', ( #16980, #357, #21370 ) ) ;
#12346 = CIRCLE ( 'NONE', #7481, 0.7619999999999294005 ) ;
#12347 = DIRECTION ( 'NONE',  ( 0.000000000000000000, 1.000000000000000000, 0.000000000000000000 ) ) ;
#12348 = ORIENTED_EDGE ( 'NONE', *, *, #12530, .F. ) ;
#12349 = VERTEX_POINT ( 'NONE', #20028 ) ;
#12350 = APPLIED_SECURITY_CLASSIFICATION_ASSIGNMENT ( #19460, ( #2608 ) ) ;
#12351 = CARTESIAN_POINT ( 'NONE',  ( 142.2400000000000091, -3660.786127253999894, 2255.774000000000342 ) ) ;
#12352 = SECURITY_CLASSIFICATION_LEVEL ( 'unclassified' ) ;
#12353 = CARTESIAN_POINT ( 'NONE',  ( 22.54063073453000143, -3694.938000000000102, 2275.763800000000174 ) ) ;
#12354 =( GEOMETRIC_REPRESENTATION_CONTEXT ( 3 ) GLOBAL_UNCERTAINTY_ASSIGNED_CONTEXT ( ( #11342 ) ) GLOBAL_UNIT_ASSIGNED_CONTEXT ( ( #3304, #1659, #27 ) ) REPRESENTATION_CONTEXT ( 'NONE', 'WORKASPACE' ) );
#12355 = CARTESIAN_POINT ( 'NONE',  ( 47.19319999999999737, -3568.700000000000273, 2260.600000000000364 ) ) ;
#12356 = EDGE_LOOP ( 'NONE', ( #22667, #4500, #6804, #21707 ) ) ;
#12357 = DIRECTION ( 'NONE',  ( -2.324635735433000053E-14, 2.336881798971000105E-14, -1.000000000000000000 ) ) ;
#12358 = FACE_BOUND ( 'NONE', #16437, .T. ) ;
#12359 = CARTESIAN_POINT ( 'NONE',  ( 0.000000000000000000, -3543.299999999999727, 2239.009999999999764 ) ) ;
#12360 = CARTESIAN_POINT ( 'NONE',  ( 12.69999999997359019, -3596.805099999930007, 2296.210799999999836 ) ) ;
#12361 = ORIENTED_EDGE ( 'NONE', *, *, #21485, .T. ) ;
#12362 = PERSON_AND_ORGANIZATION_ROLE ( 'design_owner' ) ;
#12363 = CYLINDRICAL_SURFACE ( 'NONE', #9783, 1.269999999999882334 ) ;
#12364 = AXIS2_PLACEMENT_3D ( 'NONE', #23155, #10758, #7131 ) ;
#12365 = PRODUCT_DEFINITION ( 'UNKNOWN', '', #11230, #6452 ) ;
#12366 = CARTESIAN_POINT ( 'NONE',  ( 10.10178836517258283, -3580.656260792020021, 2249.599788755271220 ) ) ;
#12367 = DIRECTION ( 'NONE',  ( 0.000000000000000000, 0.000000000000000000, 1.000000000000000000 ) ) ;
#12368 = LOCAL_TIME ( 17, 37, 43.00000000000000000, #22702 ) ;
#12369 = APPLIED_SECURITY_CLASSIFICATION_ASSIGNMENT ( #14623, ( #7499 ) ) ;
#12370 = VERTEX_POINT ( 'NONE', #108 ) ;
#12371 = DIRECTION ( 'NONE',  ( 1.000000000000000000, 0.000000000000000000, 0.000000000000000000 ) ) ;
#12372 = ADVANCED_FACE ( 'NONE', ( #18257 ), #13098, .T. ) ;
#12373 = ADVANCED_FACE ( 'NONE', ( #14867 ), #10660, .T. ) ;
#12374 = CARTESIAN_POINT ( 'NONE',  ( 0.000000000000000000, -3543.299999999999727, 2260.600000000000364 ) ) ;
#12375 = CARTESIAN_POINT ( 'NONE',  ( 127.0000000000000000, -3619.500000000000000, 2239.771999999999935 ) ) ;
#12376 = CARTESIAN_POINT ( 'NONE',  ( 10.58626199040230986, -3661.408970440582834, 2249.938111678748555 ) ) ;
#12377 = PRODUCT ( 'Roller 2', 'Roller 2', '', ( #7412 ) ) ;
#12378 = ADVANCED_FACE ( 'NONE', ( #14405 ), #2103, .T. ) ;
#12379 = DIRECTION ( 'NONE',  ( -1.000000000000000000, 0.000000000000000000, 0.000000000000000000 ) ) ;
#12380 = ORIENTED_EDGE ( 'NONE', *, *, #17292, .T. ) ;
#12381 = DIRECTION ( 'NONE',  ( 0.000000000000000000, 1.000000000000000000, 0.000000000000000000 ) ) ;
#12382 = DIRECTION ( 'NONE',  ( -1.000000000000000000, 0.000000000000000000, 0.000000000000000000 ) ) ;
#12383 = DIRECTION ( 'NONE',  ( -1.000000000000000000, -0.000000000000000000, -0.000000000000000000 ) ) ;
#12384 = CARTESIAN_POINT ( 'NONE',  ( 14.85465215501677605, -3657.647354326531513, 2248.763246533717393 ) ) ;
#12385 = EDGE_CURVE ( 'NONE', #572, #17725, #22069, .T. ) ;
#12386 = CARTESIAN_POINT ( 'NONE',  ( 136.8942325653789851, -3695.547111921297528, 2255.108514516369269 ) ) ;
#12387 = APPLIED_SECURITY_CLASSIFICATION_ASSIGNMENT ( #43, ( #23170 ) ) ;
#12388 = EDGE_LOOP ( 'NONE', ( #10798, #1646, #19641, #17561 ) ) ;
#12389 = APPLIED_APPROVAL_ASSIGNMENT ( #4060, ( #12017 ) ) ;
#12390 = CARTESIAN_POINT ( 'NONE',  ( 10.34103833421398377, -3577.903977763734019, 2250.071793175431594 ) ) ;
#12391 = ORIENTED_EDGE ( 'NONE', *, *, #3342, .F. ) ;
#12392 = CARTESIAN_POINT ( 'NONE',  ( 132.1456718464000062, -3544.321224993999749, 2260.506484774000000 ) ) ;
#12393 = EDGE_CURVE ( 'NONE', #17394, #14734, #18140, .T. ) ;
#12394 = CARTESIAN_POINT ( 'NONE',  ( 15.24000000000000021, -3660.786127253999894, 2255.774000000000342 ) ) ;
#12395 = CALENDAR_DATE ( 2026, 26, 10 ) ;
#12396 = CIRCLE ( 'NONE', #2647, 2.844799999998998796 ) ;
#12397 = DIRECTION ( 'NONE',  ( 0.000000000000000000, 0.000000000000000000, 1.000000000000000000 ) ) ;
#12398 = DIRECTION ( 'NONE',  ( 0.000000000000000000, 0.000000000000000000, 1.000000000000000000 ) ) ;
#12399 = CARTESIAN_POINT ( 'NONE',  ( 15.74606938694885550, -3657.399157459567505, 2246.629983459085906 ) ) ;
#12400 = VERTEX_POINT ( 'NONE', #16158 ) ;
#12401 = CARTESIAN_POINT ( 'NONE',  ( 95.25000000000000000, -3695.699999999999818, 2247.392000000000280 ) ) ;
#12402 = LINE ( 'NONE', #1494, #16233 ) ;
#12403 = APPLIED_APPROVAL_ASSIGNMENT ( #20937, ( #15394 ) ) ;
#12404 = CYLINDRICAL_SURFACE ( 'NONE', #19991, 0.3809999999999647002 ) ;
#12405 = ORIENTED_EDGE ( 'NONE', *, *, #21689, .F. ) ;
#12406 = CARTESIAN_POINT ( 'NONE',  ( 114.2999999999999972, -3644.899999999999636, 2239.771999999999935 ) ) ;
#12407 = EDGE_CURVE ( 'NONE', #11149, #11279, #11421, .T. ) ;
#12408 = DIRECTION ( 'NONE',  ( -0.000000000000000000, -1.000000000000000000, -0.000000000000000000 ) ) ;
#12409 = VERTEX_POINT ( 'NONE', #10883 ) ;
#12410 = CARTESIAN_POINT ( 'NONE',  ( 12.69999999999999929, -3636.327499999999873, 2290.241799999999785 ) ) ;
#12411 = AXIS2_PLACEMENT_3D ( 'NONE', #18958, #3828, #14621 ) ;
#12412 = ADVANCED_FACE ( 'NONE', ( #18029 ), #16387, .F. ) ;
#12413 = AXIS2_PLACEMENT_3D ( 'NONE', #15727, #1651, #21000 ) ;
#12414 = EDGE_CURVE ( 'NONE', #5647, #7405, #19909, .T. ) ;
#12415 = VERTEX_POINT ( 'NONE', #8174 ) ;
#12416 = DIRECTION ( 'NONE',  ( 0.000000000000000000, -1.000000000000000000, 0.000000000000000000 ) ) ;
#12417 = CARTESIAN_POINT ( 'NONE',  ( 142.4730284656999970, -3660.140000970000074, 2250.236800000000130 ) ) ;
#12418 = ORIENTED_EDGE ( 'NONE', *, *, #16235, .T. ) ;
#12419 = CARTESIAN_POINT ( 'NONE',  ( 136.8552000000000248, -3579.666931380626011, 2250.125652639312193 ) ) ;
#12420 = ORIENTED_EDGE ( 'NONE', *, *, #14245, .F. ) ;
#12421 = PERSON_AND_ORGANIZATION ( #5446, #1895 ) ;
#12422 = FACE_OUTER_BOUND ( 'NONE', #7354, .T. ) ;
#12423 = CARTESIAN_POINT ( 'NONE',  ( -6.349999999999999645, -3578.860000000000127, 2247.392000000000280 ) ) ;
#12424 = CARTESIAN_POINT ( 'NONE',  ( 110.6932000000009992, -3644.899999999999636, 2239.009999999999764 ) ) ;
#12425 = DIRECTION ( 'NONE',  ( 1.000000000000000000, 0.000000000000000000, 0.000000000000000000 ) ) ;
#12426 = VECTOR ( 'NONE', #11366, 1000.000000000000000 ) ;
#12427 = FACE_OUTER_BOUND ( 'NONE', #9091, .T. ) ;
#12428 = ORIENTED_EDGE ( 'NONE', *, *, #5855, .T. ) ;
#12429 = FACE_OUTER_BOUND ( 'NONE', #15948, .T. ) ;
#12430 = ORIENTED_EDGE ( 'NONE', *, *, #8253, .T. ) ;
#12431 = CARTESIAN_POINT ( 'NONE',  ( 4.926382664726756566, -3695.340677395856801, 2260.215245127323669 ) ) ;
#12432 = FACE_OUTER_BOUND ( 'NONE', #9514, .T. ) ;
#12433 = CIRCLE ( 'NONE', #16548, 2.844799999999961582 ) ;
#12434 = ADVANCED_FACE ( 'NONE', ( #17179 ), #22217, .T. ) ;
#12435 = EDGE_CURVE ( 'NONE', #16091, #17137, #20410, .T. ) ;
#12436 = EDGE_CURVE ( 'NONE', #17069, #14185, #7327, .T. ) ;
#12437 = FACE_OUTER_BOUND ( 'NONE', #15318, .T. ) ;
#12438 = ORIENTED_EDGE ( 'NONE', *, *, #1932, .F. ) ;
#12439 = EDGE_CURVE ( 'NONE', #6183, #10881, #4323, .T. ) ;
#12440 = CARTESIAN_POINT ( 'NONE',  ( 15.07352087697999998, -3661.081667652999840, 2257.848687205999795 ) ) ;
#12441 = AXIS2_PLACEMENT_3D ( 'NONE', #19339, #7044, #6808 ) ;
#12442 = LINE ( 'NONE', #8815, #20043 ) ;
#12443 = AXIS2_PLACEMENT_3D ( 'NONE', #21931, #15796, #3019 ) ;
#12444 = ORIENTED_EDGE ( 'NONE', *, *, #11287, .T. ) ;
#12445 = DIRECTION ( 'NONE',  ( 0.000000000000000000, 0.000000000000000000, -1.000000000000000000 ) ) ;
#12446 = DIRECTION ( 'NONE',  ( -0.000000000000000000, 1.000000000000000000, 0.000000000000000000 ) ) ;
#12447 = CARTESIAN_POINT ( 'NONE',  ( 137.8194210580677463, -3657.362480067789875, 2257.752117377573541 ) ) ;
#12448 = EDGE_CURVE ( 'NONE', #19621, #1443, #22357, .T. ) ;
#12449 = FACE_OUTER_BOUND ( 'NONE', #18584, .T. ) ;
#12450 = PERSON_AND_ORGANIZATION_ROLE ( 'classification_officer' ) ;
#12451 = CARTESIAN_POINT ( 'NONE',  ( 12.69999999999143903, -3642.377129489641902, 2296.591799999931936 ) ) ;
#12452 = PLANE ( 'NONE',  #10917 ) ;
#12453 = ORIENTED_EDGE ( 'NONE', *, *, #531, .F. ) ;
#12454 = LINE ( 'NONE', #6617, #20504 ) ;
#12455 = VECTOR ( 'NONE', #17139, 1000.000000000000000 ) ;
#12456 = ADVANCED_FACE ( 'NONE', ( #20697 ), #8056, .T. ) ;
#12457 = CARTESIAN_POINT ( 'NONE',  ( 137.2370452280314055, -3658.078236828710487, 2249.356016053515305 ) ) ;
#12458 = EDGE_CURVE ( 'NONE', #7639, #7043, #219, .T. ) ;
#12459 = VERTEX_POINT ( 'NONE', #20360 ) ;
#12460 = CIRCLE ( 'NONE', #835, 3.606800000000021100 ) ;
#12461 = CARTESIAN_POINT ( 'NONE',  ( 47.19319999999999737, -3670.300000000000182, 2259.837999999999738 ) ) ;
#12462 = TOROIDAL_SURFACE ( 'NONE', #15087, 3.606799999999999784, 0.7620000000000000107 ) ;
#12463 = ORIENTED_EDGE ( 'NONE', *, *, #3490, .T. ) ;
#12464 = ORIENTED_EDGE ( 'NONE', *, *, #19418, .F. ) ;
#12465 = ORIENTED_EDGE ( 'NONE', *, *, #2929, .T. ) ;
#12466 = DIRECTION ( 'NONE',  ( 1.000000000000000000, 0.000000000000000000, 0.000000000000000000 ) ) ;
#12467 = ORIENTED_EDGE ( 'NONE', *, *, #20599, .F. ) ;
#12468 = VERTEX_POINT ( 'NONE', #6075 ) ;
#12469 = CARTESIAN_POINT ( 'NONE',  ( 1.270000000000000018, -3694.430000000000291, 2259.329999999999927 ) ) ;
#12470 = CONTEXT_DEPENDENT_SHAPE_REPRESENTATION ( #19685, #16694 ) ;
#12471 = DIRECTION ( 'NONE',  ( -1.118034086297999961E-13, 2.590196616219000170E-13, -1.000000000000000000 ) ) ;
#12472 = DIRECTION ( 'NONE',  ( 0.000000000000000000, -1.000000000000000000, 0.000000000000000000 ) ) ;
#12473 = VERTEX_POINT ( 'NONE', #4644 ) ;
#12474 = CARTESIAN_POINT ( 'NONE',  ( 12.69999999999999929, -3654.043999999999869, 2239.391000000000076 ) ) ;
#12475 = FACE_BOUND ( 'NONE', #3407, .T. ) ;
#12476 = FACE_OUTER_BOUND ( 'NONE', #18139, .T. ) ;
#12477 = VECTOR ( 'NONE', #18892, 1000.000000000000000 ) ;
#12478 = DIRECTION ( 'NONE',  ( 0.000000000000000000, 1.000000000000000000, 0.000000000000000000 ) ) ;
#12479 = ORIENTED_EDGE ( 'NONE', *, *, #21772, .F. ) ;
#12480 = PERSON_AND_ORGANIZATION ( #5446, #1895 ) ;
#12481 = AXIS2_PLACEMENT_3D ( 'NONE', #1297, #22966, #15486 ) ;
#12482 = ORIENTED_EDGE ( 'NONE', *, *, #12075, .T. ) ;
#12483 = CARTESIAN_POINT ( 'NONE',  ( 9.855390812759999619, -3579.528596999999991, 2250.157115725000040 ) ) ;
#12484 = FACE_OUTER_BOUND ( 'NONE', #12693, .T. ) ;
#12485 = PLANE ( 'NONE',  #20931 ) ;
#12486 = ORIENTED_EDGE ( 'NONE', *, *, #17355, .F. ) ;
#12487 = CIRCLE ( 'NONE', #6894, 2.844800000000091700 ) ;
#12488 = DIRECTION ( 'NONE',  ( 0.000000000000000000, 0.000000000000000000, 1.000000000000000000 ) ) ;
#12489 = LINE ( 'NONE', #3578, #21158 ) ;
#12490 = CARTESIAN_POINT ( 'NONE',  ( 15.54479999999999862, -3639.502500000000964, 2263.571799999999712 ) ) ;
#12491 = CYLINDRICAL_SURFACE ( 'NONE', #22686, 0.3809999999999154618 ) ;
#12492 = DIRECTION ( 'NONE',  ( 0.000000000000000000, -1.000000000000000000, 0.000000000000000000 ) ) ;
#12493 = APPLICATION_CONTEXT ( 'configuration controlled 3d designs of mechanical parts and assemblies' ) ;
#12494 = CARTESIAN_POINT ( 'NONE',  ( 147.7813569001403380, -3543.300000000019736, 2259.444513955824277 ) ) ;
#12495 = ORIENTED_EDGE ( 'NONE', *, *, #10421, .F. ) ;
#12496 = DIRECTION ( 'NONE',  ( 0.000000000000000000, 1.000000000000000000, 0.000000000000000000 ) ) ;
#12497 = DIRECTION ( 'NONE',  ( -1.000000000000000000, 0.000000000000000000, 0.000000000000000000 ) ) ;
#12498 = PRODUCT_RELATED_PRODUCT_CATEGORY ( 'detail', '', ( #11987 ) ) ;
#12499 = CARTESIAN_POINT ( 'NONE',  ( 18.41499999999899728, -3599.497499999999945, 2288.971800000000258 ) ) ;
#12500 = CARTESIAN_POINT ( 'NONE',  ( 14.98249584125296430, -3657.807061604205046, 2249.020059837405825 ) ) ;
#12501 = CARTESIAN_POINT ( 'NONE',  ( 12.69999999999999929, -3659.504999999999654, 2270.760000000000218 ) ) ;
#12502 = AXIS2_PLACEMENT_3D ( 'NONE', #15691, #17434, #1613 ) ;
#12503 = CARTESIAN_POINT ( 'NONE',  ( 9.855200000000998273, -3659.504999999999654, 2256.063560000000052 ) ) ;
#12504 = ORIENTED_EDGE ( 'NONE', *, *, #15737, .T. ) ;
#12505 = EDGE_CURVE ( 'NONE', #6730, #5647, #20826, .T. ) ;
#12506 = CARTESIAN_POINT ( 'NONE',  ( 132.3005794017000198, -3544.570000000000164, 2260.390449568000349 ) ) ;
#12507 = EDGE_CURVE ( 'NONE', #952, #10748, #18705, .T. ) ;
#12508 = FACE_OUTER_BOUND ( 'NONE', #20212, .T. ) ;
#12509 = CALENDAR_DATE ( 2026, 26, 10 ) ;
#12510 = EDGE_CURVE ( 'NONE', #7881, #15010, #886, .T. ) ;
#12511 = CARTESIAN_POINT ( 'NONE',  ( 60.21459350834000190, -3694.938000000000102, 2280.170699136999701 ) ) ;
#12512 = CARTESIAN_POINT ( 'NONE',  ( 92.50679999999999836, -3644.899999999999636, 2239.771999999999935 ) ) ;
#12513 = LINE ( 'NONE', #19660, #15952 ) ;
#12514 =( BOUNDED_CURVE ( )  B_SPLINE_CURVE ( 3, ( #5126, #19526, #19412, #12143 ),
 .UNSPECIFIED., .F., .F. ) 
 B_SPLINE_CURVE_WITH_KNOTS ( ( 4, 4 ),
 ( 1.570796326272141830, 3.141592653589783346 ),
 .UNSPECIFIED. ) 
 CURVE ( )  GEOMETRIC_REPRESENTATION_ITEM ( )  RATIONAL_B_SPLINE_CURVE ( ( 1.000000000000000000, 0.8047378540011528303, 0.8047378540011528303, 1.000000000000000000 ) ) 
 REPRESENTATION_ITEM ( '' )  );
#12515 = CARTESIAN_POINT ( 'NONE',  ( 91.74479999999999791, -3644.899999999999636, 2259.837999999999738 ) ) ;
#12516 = ADVANCED_FACE ( 'NONE', ( #1010 ), #4530, .F. ) ;
#12517 = EDGE_LOOP ( 'NONE', ( #12549, #19214, #1796, #4298 ) ) ;
#12518 = DIRECTION ( 'NONE',  ( 0.000000000000000000, 0.000000000000000000, 1.000000000000000000 ) ) ;
#12519 = ORIENTED_EDGE ( 'NONE', *, *, #5347, .F. ) ;
#12520 = AXIS2_PLACEMENT_3D ( 'NONE', #10381, #15894, #8627 ) ;
#12521 = CARTESIAN_POINT ( 'NONE',  ( 95.25000000000000000, -3544.570000000000164, 2243.277199999999993 ) ) ;
#12522 = CIRCLE ( 'NONE', #2421, 3.606800000000000228 ) ;
#12523 = CARTESIAN_POINT ( 'NONE',  ( 25.39999999999999858, -3578.860000000000127, 2247.392000000000280 ) ) ;
#12524 = AXIS2_PLACEMENT_3D ( 'NONE', #4767, #22109, #4311 ) ;
#12525 = EDGE_LOOP ( 'NONE', ( #9434, #4968, #14755, #21981 ) ) ;
#12526 = DIRECTION ( 'NONE',  ( 0.000000000000000000, 0.000000000000000000, -1.000000000000000000 ) ) ;
#12527 = EDGE_LOOP ( 'NONE', ( #16757, #15580, #1536, #21454 ) ) ;
#12528 = CARTESIAN_POINT ( 'NONE',  ( 142.5418463402332634, -3695.591362400878552, 2255.017959195591175 ) ) ;
#12529 = ORIENTED_EDGE ( 'NONE', *, *, #690, .T. ) ;
#12530 = EDGE_CURVE ( 'NONE', #185, #13091, #22335, .T. ) ;
#12531 = CARTESIAN_POINT ( 'NONE',  ( 137.4922034527655512, -3581.289558263637446, 2248.872981960140805 ) ) ;
#12532 = VECTOR ( 'NONE', #22076, 1000.000000000000114 ) ;
#12533 = ORIENTED_EDGE ( 'NONE', *, *, #17556, .T. ) ;
#12534 = CARTESIAN_POINT ( 'NONE',  ( 3.048000000000000043, -3694.938000000000102, 2229.612000000000080 ) ) ;
#12535 = TOROIDAL_SURFACE ( 'NONE', #6200, 3.606799999999999784, 0.7620000000000000107 ) ;
#12536 = ADVANCED_FACE ( 'NONE', ( #11559 ), #15547, .T. ) ;
#12537 = CALENDAR_DATE ( 2026, 26, 10 ) ;
#12539 = ADVANCED_FACE ( 'NONE', ( #13676 ), #18482, .T. ) ;
#12538 = VECTOR ( 'NONE', #1748, 1000.000000000000000 ) ;
#12540 = AXIS2_PLACEMENT_3D ( 'NONE', #21031, #15517, #3322 ) ;
#12541 = DIRECTION ( 'NONE',  ( 1.000000000000000000, -0.000000000000000000, -0.000000000000000000 ) ) ;
#12542 = CARTESIAN_POINT ( 'NONE',  ( -0.7620000000000000107, -3544.061999999999898, 2253.487999999999829 ) ) ;
#12543 = DIRECTION ( 'NONE',  ( 1.000000000000000000, 0.000000000000000000, 0.000000000000000000 ) ) ;
#12544 = LINE ( 'NONE', #8797, #7243 ) ;
#12545 = DIRECTION ( 'NONE',  ( 0.000000000000000000, 0.000000000000000000, -1.000000000000000000 ) ) ;
#12546 = EDGE_LOOP ( 'NONE', ( #18633, #22895, #14485 ) ) ;
#12547 = CARTESIAN_POINT ( 'NONE',  ( 134.6666709697134650, -3576.788180027481758, 2245.442509231440454 ) ) ;
#12548 = CARTESIAN_POINT ( 'NONE',  ( 139.6999999999999886, -3576.320000000000164, 2270.760000000000218 ) ) ;
#12549 = ORIENTED_EDGE ( 'NONE', *, *, #18815, .F. ) ;
#12550 = AXIS2_PLACEMENT_3D ( 'NONE', #18428, #13386, #838 ) ;
#12551 = CARTESIAN_POINT ( 'NONE',  ( 9.855200508393231473, -3579.494999998446929, 2257.962940200991852 ) ) ;
#12552 = CARTESIAN_POINT ( 'NONE',  ( 137.3683132029000262, -3658.158799999999701, 2239.391000000000076 ) ) ;
#12553 = VECTOR ( 'NONE', #22935, 1000.000000000000114 ) ;
#12554 = DIRECTION ( 'NONE',  ( -1.000000000000000000, 0.000000000000000000, 0.000000000000000000 ) ) ;
#12555 = AXIS2_PLACEMENT_3D ( 'NONE', #15962, #3415, #10567 ) ;
#12556 = ORIENTED_EDGE ( 'NONE', *, *, #21878, .F. ) ;
#12557 = CARTESIAN_POINT ( 'NONE',  ( 14.27720943205999937, -3661.878154638000524, 2257.704281108000032 ) ) ;
#12558 = CARTESIAN_POINT ( 'NONE',  ( 88.90000000000000568, -3644.899999999999636, 2239.771999999999935 ) ) ;
#12559 = EDGE_LOOP ( 'NONE', ( #10761, #7474, #20526, #9823 ) ) ;
#12560 = CARTESIAN_POINT ( 'NONE',  ( 139.6999999999999886, -3661.409999999999400, 2270.760000000000218 ) ) ;
#12561 = CARTESIAN_POINT ( 'NONE',  ( 10.92596159350999940, -3641.734223874999770, 2279.676121195000178 ) ) ;
#12562 = EDGE_CURVE ( 'NONE', #14878, #22087, #16990, .T. ) ;
#12563 = FACE_BOUND ( 'NONE', #12003, .T. ) ;
#12564 = LINE ( 'NONE', #19720, #9606 ) ;
#12565 = PERSON_AND_ORGANIZATION_ROLE ( 'design_supplier' ) ;
#12566 = ORIENTED_EDGE ( 'NONE', *, *, #5088, .T. ) ;
#12567 = CARTESIAN_POINT ( 'NONE',  ( 142.0316867971999955, -3580.841199999999844, 2242.820000000000164 ) ) ;
#12568 = CARTESIAN_POINT ( 'NONE',  ( 9.842801829194641527, -3695.607672421227107, 2254.979458605150285 ) ) ;
#12569 = EDGE_LOOP ( 'NONE', ( #21830, #1681, #8927, #22574 ) ) ;
#12570 = CARTESIAN_POINT ( 'NONE',  ( 142.0316867971999955, -3660.851200000000063, 2239.391000000000076 ) ) ;
#12571 = VECTOR ( 'NONE', #12963, 1000.000000000000000 ) ;
#12572 = TOROIDAL_SURFACE ( 'NONE', #20076, 1.905000000000000027, 1.270000000000000018 ) ;
#12573 = ADVANCED_FACE ( 'NONE', ( #9693 ), #22610, .T. ) ;
#12574 = CARTESIAN_POINT ( 'NONE',  ( 0.7620000000000000107, -3694.938000000000102, 2275.001800000000003 ) ) ;
#12575 = CIRCLE ( 'NONE', #1717, 2.844799999999994444 ) ;
#12576 = EDGE_CURVE ( 'NONE', #4163, #9004, #16252, .T. ) ;
#12577 = AXIS2_PLACEMENT_3D ( 'NONE', #14285, #21431, #3721 ) ;
#12578 = ORIENTED_EDGE ( 'NONE', *, *, #21463, .T. ) ;
#12579 = AXIS2_PLACEMENT_3D ( 'NONE', #19351, #358, #22210 ) ;
#12580 = CARTESIAN_POINT ( 'NONE',  ( 142.4126867973300534, -3577.928829547225178, 2239.009999999999764 ) ) ;
#12581 = ORIENTED_EDGE ( 'NONE', *, *, #13517, .T. ) ;
#12582 = ORIENTED_EDGE ( 'NONE', *, *, #6126, .T. ) ;
#12583 = EDGE_CURVE ( 'NONE', #8369, #11141, #8527, .T. ) ;
#12584 = ORIENTED_EDGE ( 'NONE', *, *, #7004, .F. ) ;
#12585 = CARTESIAN_POINT ( 'NONE',  ( 12.69999999999999929, -3599.497499999999945, 2296.591799999999694 ) ) ;
#12586 = ORIENTED_EDGE ( 'NONE', *, *, #19769, .T. ) ;
#12587 = EDGE_LOOP ( 'NONE', ( #10009, #375, #8490, #6738 ) ) ;
#12588 = CARTESIAN_POINT ( 'NONE',  ( 9.855199999999999960, -3579.494999999999891, 2272.030000000000200 ) ) ;
#12589 = CIRCLE ( 'NONE', #4717, 3.175000000000149925 ) ;
#12590 = APPROVAL_ROLE ( '' ) ;
#12591 = AXIS2_PLACEMENT_3D ( 'NONE', #9770, #16914, #859 ) ;
#12592 = FACE_OUTER_BOUND ( 'NONE', #9136, .T. ) ;
#12593 = EDGE_CURVE ( 'NONE', #1809, #118, #2319, .T. ) ;
#12594 = ORIENTED_EDGE ( 'NONE', *, *, #14152, .T. ) ;
#12595 = AXIS2_PLACEMENT_3D ( 'NONE', #13393, #14813, #9750 ) ;
#12596 = CARTESIAN_POINT ( 'NONE',  ( 151.1299999999999955, -3578.860000000000127, 2244.547199999999975 ) ) ;
#12597 = EDGE_CURVE ( 'NONE', #13004, #1122, #22911, .T. ) ;
#12598 = DIRECTION ( 'NONE',  ( -0.000000000000000000, 1.000000000000000000, 0.000000000000000000 ) ) ;
#12599 = CARTESIAN_POINT ( 'NONE',  ( 7.048736936763374317, -3580.386377785101104, 2244.978268890040454 ) ) ;
#12600 = PLANE ( 'NONE',  #18222 ) ;
#12601 = VECTOR ( 'NONE', #20686, 1000.000000000000000 ) ;
#12602 = COORDINATED_UNIVERSAL_TIME_OFFSET ( 0, 0, .AHEAD. ) ;
#12603 = ORIENTED_EDGE ( 'NONE', *, *, #6677, .F. ) ;
#12604 = CARTESIAN_POINT ( 'NONE',  ( 131.7384701241167022, -3543.369601860909370, 2259.744672092661858 ) ) ;
#12605 = ORIENTED_EDGE ( 'NONE', *, *, #13453, .F. ) ;
#12606 = CARTESIAN_POINT ( 'NONE',  ( 66.34479999999999222, -3594.099999999999909, 2259.837999999999738 ) ) ;
#12607 = EDGE_CURVE ( 'NONE', #15790, #16219, #9148, .T. ) ;
#12608 = CARTESIAN_POINT ( 'NONE',  ( 66.34479999999999222, -3644.899999999999636, 2261.869999999999891 ) ) ;
#12609 = ORIENTED_EDGE ( 'NONE', *, *, #16735, .F. ) ;
#12610 = CARTESIAN_POINT ( 'NONE',  ( 139.6999999999999886, -3659.504999999999654, 2270.760000000000218 ) ) ;
#12611 = AXIS2_PLACEMENT_3D ( 'NONE', #2394, #20529, #20319 ) ;
#12612 = CARTESIAN_POINT ( 'NONE',  ( 15.54479999999999862, -3599.497499999999945, 2263.571799999999712 ) ) ;
#12613 = LINE ( 'NONE', #14256, #11838 ) ;
#12614 = AXIS2_PLACEMENT_3D ( 'NONE', #15688, #15451, #15572 ) ;
#12615 = DIRECTION ( 'NONE',  ( 1.000000000000000000, 0.000000000000000000, 0.000000000000000000 ) ) ;
#12616 = VECTOR ( 'NONE', #22407, 1000.000000000000000 ) ;
#12617 = FACE_OUTER_BOUND ( 'NONE', #2269, .T. ) ;
#12618 = DIRECTION ( 'NONE',  ( -1.000000000000000000, 0.000000000000000000, 0.000000000000000000 ) ) ;
#12619 = EDGE_LOOP ( 'NONE', ( #16860, #3553 ) ) ;
#12620 = CARTESIAN_POINT ( 'NONE',  ( 147.4427463453449718, -3695.258941567852162, 2260.292568422380100 ) ) ;
#12621 = DIRECTION ( 'NONE',  ( -1.000000000000000000, 0.000000000000000000, 0.000000000000000000 ) ) ;
#12622 = CARTESIAN_POINT ( 'NONE',  ( 15.18950216437265333, -3660.942314744880605, 2239.010000000072068 ) ) ;
#12623 = CARTESIAN_POINT ( 'NONE',  ( 142.5448000000000093, -3579.282532373467347, 2250.213677521736827 ) ) ;
#12624 = CARTESIAN_POINT ( 'NONE',  ( 142.4037490354116926, -3543.632335306846016, 2255.363857416194605 ) ) ;
#12625 = CARTESIAN_POINT ( 'NONE',  ( 136.6529205195000145, -3695.699999999999818, 2254.503999999999905 ) ) ;
#12626 = VERTEX_POINT ( 'NONE', #10621 ) ;
#12627 = CARTESIAN_POINT ( 'NONE',  ( 50.79999999999999716, -3568.700000000000273, 2259.837999999999738 ) ) ;
#12628 = EDGE_LOOP ( 'NONE', ( #15248, #4078, #18631, #5928, #21559, #19497, #17745, #1370 ) ) ;
#12629 = CARTESIAN_POINT ( 'NONE',  ( 12.70000000000000107, -3590.289999999999964, 2275.817139999999654 ) ) ;
#12630 = CARTESIAN_POINT ( 'NONE',  ( 9.998032641076921578, -3543.639179023070028, 2255.368368629587167 ) ) ;
#12631 = DATE_TIME_ROLE ( 'classification_date' ) ;
#12632 = DIRECTION ( 'NONE',  ( 0.7249994335957196112, -1.571266676791983932E-13, 0.6887494619133185392 ) ) ;
#12633 = TOROIDAL_SURFACE ( 'NONE', #4033, 6.477000000001000402, 0.7620000000000000107 ) ;
#12634 = CARTESIAN_POINT ( 'NONE',  ( 3.175000000094025054, -3694.938000000000102, 2275.001800000090952 ) ) ;
#12635 = CARTESIAN_POINT ( 'NONE',  ( 116.8400000000000034, -3568.700000000000273, 2247.392000000000280 ) ) ;
#12636 = CARTESIAN_POINT ( 'NONE',  ( 151.4000000000000057, -3544.570000000000164, 2259.329999999999927 ) ) ;
#12637 = DIRECTION ( 'NONE',  ( -0.000000000000000000, 1.000000000000000000, 0.000000000000000000 ) ) ;
#12638 = VERTEX_POINT ( 'NONE', #19183 ) ;
#12639 = DIRECTION ( 'NONE',  ( 0.000000000000000000, -1.000000000000000000, 0.000000000000000000 ) ) ;
#12640 = TOROIDAL_SURFACE ( 'NONE', #22354, 3.606799999998999695, 0.7620000000000000107 ) ;
#12641 = EDGE_CURVE ( 'NONE', #14185, #17069, #14017, .T. ) ;
#12642 = CARTESIAN_POINT ( 'NONE',  ( 9.918918857905000053, -3638.876466522000101, 2279.464085466000142 ) ) ;
#12643 = ORIENTED_EDGE ( 'NONE', *, *, #13712, .T. ) ;
#12644 = DIRECTION ( 'NONE',  ( -1.000000000000000000, 0.000000000000000000, 0.000000000000000000 ) ) ;
#12645 = ORIENTED_EDGE ( 'NONE', *, *, #16554, .F. ) ;
#12646 = CARTESIAN_POINT ( 'NONE',  ( 142.3028687989565526, -3695.048176945954765, 2255.616383243821019 ) ) ;
#12647 = DIRECTION ( 'NONE',  ( 0.000000000000000000, 0.000000000000000000, 1.000000000000000000 ) ) ;
#12648 = EDGE_LOOP ( 'NONE', ( #143, #4319, #5578, #18513 ) ) ;
#12649 = CARTESIAN_POINT ( 'NONE',  ( 137.1922541308920813, -3580.838518559781278, 2249.436926605831559 ) ) ;
#12650 = ORIENTED_EDGE ( 'NONE', *, *, #7703, .F. ) ;
#12651 = DIRECTION ( 'NONE',  ( -1.000000000000000000, 0.000000000000000000, 0.000000000000000000 ) ) ;
#12652 =( BOUNDED_CURVE ( )  B_SPLINE_CURVE ( 3, ( #22419, #11639, #20665, #6050 ),
 .UNSPECIFIED., .F., .T. ) 
 B_SPLINE_CURVE_WITH_KNOTS ( ( 4, 4 ),
 ( 3.673835071120097305E-14, 1.570796326491086026 ),
 .UNSPECIFIED. ) 
 CURVE ( )  GEOMETRIC_REPRESENTATION_ITEM ( )  RATIONAL_B_SPLINE_CURVE ( ( 1.000000000000000000, 0.8047378541959824272, 0.8047378541959824272, 1.000000000000000000 ) ) 
 REPRESENTATION_ITEM ( '' )  );
#12653 = APPROVAL_DATE_TIME ( #14070, #5631 ) ;
#12654 = AXIS2_PLACEMENT_3D ( 'NONE', #718, #16992, #15024 ) ;
#12655 = CARTESIAN_POINT ( 'NONE',  ( 142.0316867971266390, -3660.851200000091012, 2239.391000000000076 ) ) ;
#12656 = CARTESIAN_POINT ( 'NONE',  ( 116.8400000000000034, -3568.700000000000273, 2244.547199999999975 ) ) ;
#12657 = APPROVAL ( #433, 'UNSPECIFIED' ) ;
#12658 = DIRECTION ( 'NONE',  ( 0.000000000000000000, 0.000000000000000000, 1.000000000000000000 ) ) ;
#12659 = CARTESIAN_POINT ( 'NONE',  ( 141.8559770206331621, -3577.638865271226223, 2249.961452083505264 ) ) ;
#12660 = ORIENTED_EDGE ( 'NONE', *, *, #15533, .F. ) ;
#12661 = CARTESIAN_POINT ( 'NONE',  ( 134.1130506821819779, -3578.283485894974547, 2244.602361446803570 ) ) ;
#12662 = EDGE_CURVE ( 'NONE', #3774, #6875, #7272, .T. ) ;
#12663 = ORIENTED_EDGE ( 'NONE', *, *, #3476, .F. ) ;
#12664 = FACE_OUTER_BOUND ( 'NONE', #12914, .T. ) ;
#12665 = ORIENTED_EDGE ( 'NONE', *, *, #1334, .F. ) ;
#12666 = EDGE_CURVE ( 'NONE', #9312, #3779, #14027, .T. ) ;
#12667 = CARTESIAN_POINT ( 'NONE',  ( 12.15052771711000013, -3582.290804947000197, 2257.605120077999800 ) ) ;
#12668 = VERTEX_POINT ( 'NONE', #1594 ) ;
#12669 = CARTESIAN_POINT ( 'NONE',  ( 20.32000000000000028, -3670.300000000000182, 2289.213099999999940 ) ) ;
#12670 = EDGE_CURVE ( 'NONE', #17227, #15883, #17000, .T. ) ;
#12671 = VERTEX_POINT ( 'NONE', #21183 ) ;
#12672 = DIRECTION ( 'NONE',  ( -0.6723379328325259641, -0.7402443543009875615, 0.000000000000000000 ) ) ;
#12673 = CARTESIAN_POINT ( 'NONE',  ( 142.4126867972053674, -3581.061170452544502, 2239.009999999999764 ) ) ;
#12674 = AXIS2_PLACEMENT_3D ( 'NONE', #13331, #2657, #2552 ) ;
#12675 = ORIENTED_EDGE ( 'NONE', *, *, #22429, .F. ) ;
#12676 = DIRECTION ( 'NONE',  ( 0.000000000000000000, 0.000000000000000000, 1.000000000000000000 ) ) ;
#12677 = CARTESIAN_POINT ( 'NONE',  ( 10.46820691843999995, -3641.276459549999799, 2279.591867610000008 ) ) ;
#12678 =( NAMED_UNIT ( * ) PLANE_ANGLE_UNIT ( ) SI_UNIT ( $, .RADIAN. ) );
#12679 = DIRECTION ( 'NONE',  ( 0.000000000000000000, 0.000000000000000000, 1.000000000000000000 ) ) ;
#12680 = B_SPLINE_CURVE_WITH_KNOTS ( 'NONE', 3,
 ( #4948, #12213, #21245, #3182, #2954, #17351, #13976, #10216, #12094, #15732 ),
 .UNSPECIFIED., .F., .F.,
 ( 4, 2, 1, 1, 2, 4 ),
 ( 0.000000000000000000, 0.06250000000002454981, 0.1250000000000490996, 0.2500000000000422440, 0.5000000000000285327, 1.000000000000000000 ),
 .UNSPECIFIED. ) ;
#12681 = EDGE_CURVE ( 'NONE', #14851, #10901, #22221, .T. ) ;
#12682 = DIRECTION ( 'NONE',  ( 0.000000000000000000, 0.000000000000000000, -1.000000000000000000 ) ) ;
#12683 = COORDINATED_UNIVERSAL_TIME_OFFSET ( 0, 0, .AHEAD. ) ;
#12684 = CARTESIAN_POINT ( 'NONE',  ( 9.987313202835000681, -3637.936329547000241, 2296.591799999999694 ) ) ;
#12685 = CARTESIAN_POINT ( 'NONE',  ( 9.738066884983357596, -3695.684982104192841, 2254.716481487530018 ) ) ;
#12686 = EDGE_LOOP ( 'NONE', ( #3690, #11551 ) ) ;
#12687 = CARTESIAN_POINT ( 'NONE',  ( 18.07271388913700250, -3581.449656630049049, 2246.178647457765692 ) ) ;
#12688 = ADVANCED_FACE ( 'NONE', ( #6770 ), #1722, .T. ) ;
#12689 = CARTESIAN_POINT ( 'NONE',  ( 137.6157805523781690, -3657.568573254816783, 2248.609408014333439 ) ) ;
#12690 = ORIENTED_EDGE ( 'NONE', *, *, #16662, .F. ) ;
#12691 = AXIS2_PLACEMENT_3D ( 'NONE', #15411, #13888, #990 ) ;
#12692 = CARTESIAN_POINT ( 'NONE',  ( 140.1748344546939506, -3662.310676981497636, 2249.230826604551567 ) ) ;
#12693 = EDGE_LOOP ( 'NONE', ( #15172, #12717, #18747, #18907 ) ) ;
#12694 = ORIENTED_EDGE ( 'NONE', *, *, #5643, .F. ) ;
#12695 = EDGE_CURVE ( 'NONE', #18837, #8533, #14388, .T. ) ;
#12696 = DIRECTION ( 'NONE',  ( -1.000000000000000000, 0.000000000000000000, 0.000000000000000000 ) ) ;
#12697 = VERTEX_POINT ( 'NONE', #5006 ) ;
#12698 = ORIENTED_EDGE ( 'NONE', *, *, #7998, .F. ) ;
#12699 = CARTESIAN_POINT ( 'NONE',  ( 142.2400000000000091, -3660.786127253999894, 2255.774000000000342 ) ) ;
#12700 = DATE_AND_TIME ( #5568, #19512 ) ;
#12701 = CARTESIAN_POINT ( 'NONE',  ( 139.6999999999999886, -3662.679999999999836, 2270.760000000000218 ) ) ;
#12702 = ADVANCED_BREP_SHAPE_REPRESENTATION ( '', ( #21472, #5611 ), #9349 ) ;
#12703 = DIRECTION ( 'NONE',  ( -1.000000000000000000, 0.000000000000000000, 0.000000000000000000 ) ) ;
#12704 = VECTOR ( 'NONE', #4867, 1000.000000000000000 ) ;
#12705 = EDGE_CURVE ( 'NONE', #923, #10278, #164, .T. ) ;
#12706 = ORIENTED_EDGE ( 'NONE', *, *, #18877, .F. ) ;
#12707 = ADVANCED_FACE ( 'NONE', ( #7114 ), #5238, .T. ) ;
#12708 = DIRECTION ( 'NONE',  ( 0.000000000000000000, 0.000000000000000000, 1.000000000000000000 ) ) ;
#12709 = CARTESIAN_POINT ( 'NONE',  ( -5.588000000000000078, -3660.140000000000327, 2247.392000000000280 ) ) ;
#12710 = CARTESIAN_POINT ( 'NONE',  ( 7.375511700031431417, -3581.571545880435679, 2246.524605943541246 ) ) ;
#12711 = CIRCLE ( 'NONE', #15314, 5.460999999999938126 ) ;
#12712 = PERSON_AND_ORGANIZATION_ROLE ( 'design_supplier' ) ;
#12713 = EDGE_LOOP ( 'NONE', ( #3648, #6568, #10409, #5786 ) ) ;
#12714 = CARTESIAN_POINT ( 'NONE',  ( 12.70000000028310616, -3576.362659094871105, 2239.009999999999764 ) ) ;
#12715 = ORIENTED_EDGE ( 'NONE', *, *, #15817, .T. ) ;
#12716 = LINE ( 'NONE', #14826, #2536 ) ;
#12717 = ORIENTED_EDGE ( 'NONE', *, *, #9997, .F. ) ;
#12718 = EDGE_CURVE ( 'NONE', #16380, #16556, #11915, .T. ) ;
#12719 = DIRECTION ( 'NONE',  ( 0.000000000000000000, 0.000000000000000000, 1.000000000000000000 ) ) ;
#12720 = APPLIED_APPROVAL_ASSIGNMENT ( #7921, ( #22796 ) ) ;
#12721 = CARTESIAN_POINT ( 'NONE',  ( 12.69999999999999929, -3604.958499999999731, 2290.241799999999785 ) ) ;
#12722 = CIRCLE ( 'NONE', #22420, 0.7619999999999294005 ) ;
#12723 = DIRECTION ( 'NONE',  ( 0.000000000000000000, 1.000000000000000000, 0.000000000000000000 ) ) ;
#12724 = DIRECTION ( 'NONE',  ( 7.422379454677999805E-13, -1.000000000000000000, 4.288485907146999317E-12 ) ) ;
#12725 = CYLINDRICAL_SURFACE ( 'NONE', #9570, 2.844799999999999773 ) ;
#12726 = VERTEX_POINT ( 'NONE', #15551 ) ;
#12727 = CARTESIAN_POINT ( 'NONE',  ( 147.3506313851963228, -3694.866442831903896, 2260.523303096903874 ) ) ;
#12728 = CARTESIAN_POINT ( 'NONE',  ( 12.69999999999999929, -3639.502500000000055, 2264.841800000000148 ) ) ;
#12729 = CARTESIAN_POINT ( 'NONE',  ( 1.270000000000000018, -3544.570000000000164, 2239.009999999999764 ) ) ;
#12730 = EDGE_CURVE ( 'NONE', #11858, #5217, #17407, .T. ) ;
#12731 = CARTESIAN_POINT ( 'NONE',  ( 54.40679999999999694, -3670.300000000000182, 2260.600000000000364 ) ) ;
#12732 = CARTESIAN_POINT ( 'NONE',  ( 142.5947367361206943, -3543.355825690155598, 2254.886265305463439 ) ) ;
#12733 = DIRECTION ( 'NONE',  ( 0.000000000000000000, 1.000000000000000000, 0.000000000000000000 ) ) ;
#12734 = CARTESIAN_POINT ( 'NONE',  ( 7.827395171519881067, -3576.508546973163902, 2245.790855086235297 ) ) ;
#12735 = VERTEX_POINT ( 'NONE', #16244 ) ;
#12737 = CIRCLE ( 'NONE', #389, 0.7619999999999294005 ) ;
#12736 = PERSON_AND_ORGANIZATION ( #5446, #1895 ) ;
#12738 = CARTESIAN_POINT ( 'NONE',  ( 41.70680000000000121, -3644.899999999999636, 2260.600000000000364 ) ) ;
#12739 = TOROIDAL_SURFACE ( 'NONE', #21684, 3.606799999999999784, 0.7620000000000000107 ) ;
#12740 =( GEOMETRIC_REPRESENTATION_CONTEXT ( 3 ) GLOBAL_UNCERTAINTY_ASSIGNED_CONTEXT ( ( #2448 ) ) GLOBAL_UNIT_ASSIGNED_CONTEXT ( ( #7409, #7626, #20287 ) ) REPRESENTATION_CONTEXT ( 'NONE', 'WORKASPACE' ) );
#12741 = DIRECTION ( 'NONE',  ( -1.297627797025000031E-12, -1.000000000000000000, 0.000000000000000000 ) ) ;
#12742 = SECURITY_CLASSIFICATION_LEVEL ( 'unclassified' ) ;
#12743 = LINE ( 'NONE', #16031, #18421 ) ;
#12744 = FACE_OUTER_BOUND ( 'NONE', #20922, .T. ) ;
#12745 = AXIS2_PLACEMENT_3D ( 'NONE', #15847, #17479, #8585 ) ;
#12746 = EDGE_CURVE ( 'NONE', #21153, #10346, #7456, .T. ) ;
#12747 = ADVANCED_FACE ( 'NONE', ( #14611 ), #8778, .T. ) ;
#12748 = DIRECTION ( 'NONE',  ( -1.000000000000000000, -2.186138625658999988E-13, 0.000000000000000000 ) ) ;
#12749 = LINE ( 'NONE', #21660, #1637 ) ;
#12750 = EDGE_LOOP ( 'NONE', ( #19356, #16022, #22316, #4737 ) ) ;
#12751 = CARTESIAN_POINT ( 'NONE',  ( 12.69999999999999929, -3570.287499999999909, 2268.705139999999574 ) ) ;
#12752 = CARTESIAN_POINT ( 'NONE',  ( 12.70000000000000107, -3570.287499999999909, 2279.817639999999756 ) ) ;
#12753 = ORIENTED_EDGE ( 'NONE', *, *, #12865, .F. ) ;
#12754 = LOCAL_TIME ( 17, 37, 43.00000000000000000, #1378 ) ;
#12755 = CYLINDRICAL_SURFACE ( 'NONE', #578, 2.844800000000091700 ) ;
#12756 = LOCAL_TIME ( 17, 37, 43.00000000000000000, #205 ) ;
#12757 = CIRCLE ( 'NONE', #11616, 2.844799999999009010 ) ;
#12758 = ORIENTED_EDGE ( 'NONE', *, *, #17525, .T. ) ;
#12759 = CARTESIAN_POINT ( 'NONE',  ( 142.4037675250975781, -3695.367664690104903, 2255.363864802005537 ) ) ;
#12760 = CARTESIAN_POINT ( 'NONE',  ( 137.3683132029985927, -3578.148799999858966, 2239.391000000000076 ) ) ;
#12761 = ORIENTED_EDGE ( 'NONE', *, *, #11861, .F. ) ;
#12762 = PRODUCT ( 'Screw 5', 'Screw 5', '', ( #12011 ) ) ;
#12763 = CARTESIAN_POINT ( 'NONE',  ( 137.5699719362845883, -3581.380703542814899, 2248.710691103632143 ) ) ;
#12764 = EDGE_LOOP ( 'NONE', ( #13704, #20163 ) ) ;
#12765 = CARTESIAN_POINT ( 'NONE',  ( 9.394261469307407353, -3695.700000000027103, 2281.667430734552454 ) ) ;
#12766 = PERSON_AND_ORGANIZATION_ROLE ( 'classification_officer' ) ;
#12767 = APPLICATION_CONTEXT ( 'configuration controlled 3d designs of mechanical parts and assemblies' ) ;
#12768 = CARTESIAN_POINT ( 'NONE',  ( 25.39999999999999858, -3578.860000000000127, 2250.236800000000130 ) ) ;
#12769 = CYLINDRICAL_SURFACE ( 'NONE', #5101, 0.3809999999999154618 ) ;
#12770 = DIRECTION ( 'NONE',  ( 0.000000000000000000, 0.000000000000000000, -1.000000000000000000 ) ) ;
#12771 = DIRECTION ( 'NONE',  ( 0.000000000000000000, -1.000000000000000000, 0.000000000000000000 ) ) ;
#12772 = CARTESIAN_POINT ( 'NONE',  ( 141.8954864283250572, -3577.685780687507759, 2249.983218200938154 ) ) ;
#12773 = EDGE_LOOP ( 'NONE', ( #7334, #13257, #2403, #6425 ) ) ;
#12774 = AXIS2_PLACEMENT_3D ( 'NONE', #12127, #2879, #21043 ) ;
#12775 = CARTESIAN_POINT ( 'NONE',  ( 134.8860662734080051, -3576.414507136522843, 2245.937534930719721 ) ) ;
#12776 = CIRCLE ( 'NONE', #7908, 1.904999999999823501 ) ;
#12777 = EDGE_LOOP ( 'NONE', ( #7718, #18538, #3744, #21435 ) ) ;
#12778 = LINE ( 'NONE', #3872, #14799 ) ;
#12779 = ORIENTED_EDGE ( 'NONE', *, *, #9315, .T. ) ;
#12780 = FACE_OUTER_BOUND ( 'NONE', #19191, .T. ) ;
#12781 = CARTESIAN_POINT ( 'NONE',  ( 139.6999999999999886, -3582.670000000000073, 2270.760000000000218 ) ) ;
#12782 = ORIENTED_EDGE ( 'NONE', *, *, #7283, .T. ) ;
#12783 = LINE ( 'NONE', #1887, #15028 ) ;
#12784 = DIRECTION ( 'NONE',  ( -1.000000000000000000, 0.000000000000000000, 2.324635735433000053E-14 ) ) ;
#12785 = ORIENTED_EDGE ( 'NONE', *, *, #21741, .T. ) ;
#12786 = PRODUCT_DEFINITION ( 'UNKNOWN', '', #10138, #11831 ) ;
#12787 = DIRECTION ( 'NONE',  ( 0.000000000000000000, 0.000000000000000000, 1.000000000000000000 ) ) ;
#12788 = FACE_BOUND ( 'NONE', #16394, .T. ) ;
#12789 =( NAMED_UNIT ( * ) PLANE_ANGLE_UNIT ( ) SI_UNIT ( $, .RADIAN. ) );
#12790 = DIRECTION ( 'NONE',  ( 0.000000000000000000, -1.000000000000000000, 0.000000000000000000 ) ) ;
#12792 = DIRECTION ( 'NONE',  ( -1.000000000000000000, 0.000000000000000000, 0.000000000000000000 ) ) ;
#12791 = AXIS2_PLACEMENT_3D ( 'NONE', #4380, #11515, #9653 ) ;
#12793 = COORDINATED_UNIVERSAL_TIME_OFFSET ( 0, 0, .AHEAD. ) ;
#12794 = AXIS2_PLACEMENT_3D ( 'NONE', #11147, #141, #9390 ) ;
#12795 = ADVANCED_FACE ( 'NONE', ( #2071 ), #9102, .T. ) ;
#12796 = CARTESIAN_POINT ( 'NONE',  ( 1.270000000000000018, -3543.299999999999727, 2259.329999999999927 ) ) ;
#12797 = CARTESIAN_POINT ( 'NONE',  ( 142.0316867971999955, -3580.841199999999844, 2242.820000000000164 ) ) ;
#12798 = ORIENTED_EDGE ( 'NONE', *, *, #22900, .F. ) ;
#12800 = EDGE_CURVE ( 'NONE', #4712, #15879, #17755, .T. ) ;
#12799 = FACE_OUTER_BOUND ( 'NONE', #598, .T. ) ;
#12801 = EDGE_CURVE ( 'NONE', #10748, #16863, #7345, .T. ) ;
#12802 = CARTESIAN_POINT ( 'NONE',  ( 137.7992377516491729, -3657.388364312606882, 2248.114380174669350 ) ) ;
#12803 = ORIENTED_EDGE ( 'NONE', *, *, #1625, .F. ) ;
#12804 = EDGE_LOOP ( 'NONE', ( #9779, #1427 ) ) ;
#12805 = CIRCLE ( 'NONE', #18778, 5.460999999999938126 ) ;
#12806 = CARTESIAN_POINT ( 'NONE',  ( 138.7492288098038955, -3662.186786022434262, 2249.367902486606908 ) ) ;
#12807 = EDGE_CURVE ( 'NONE', #16889, #18145, #9522, .T. ) ;
#12808 = ORIENTED_EDGE ( 'NONE', *, *, #3409, .F. ) ;
#12809 = CIRCLE ( 'NONE', #14690, 0.3809999999999647002 ) ;
#12810 = ORIENTED_EDGE ( 'NONE', *, *, #13274, .F. ) ;
#12811 = VECTOR ( 'NONE', #18952, 1000.000000000000000 ) ;
#12812 = CARTESIAN_POINT ( 'NONE',  ( 9.855199999999999960, -3599.497499999999945, 2288.971800000000258 ) ) ;
#12813 = ORIENTED_EDGE ( 'NONE', *, *, #1967, .T. ) ;
#12814 = ORIENTED_EDGE ( 'NONE', *, *, #8238, .T. ) ;
#12815 = CARTESIAN_POINT ( 'NONE',  ( 95.25000000000000000, -3670.300000000000182, 2247.392000000000280 ) ) ;
#12816 = EDGE_CURVE ( 'NONE', #2862, #1856, #12891, .T. ) ;
#12817 = CARTESIAN_POINT ( 'NONE',  ( -12.69999999999999929, -3658.573829546965044, 2244.679313203020683 ) ) ;
#12818 = ORIENTED_EDGE ( 'NONE', *, *, #13712, .F. ) ;
#12819 = CARTESIAN_POINT ( 'NONE',  ( 12.69999999999999929, -3639.502500000000055, 2296.591799999999694 ) ) ;
#12820 = CARTESIAN_POINT ( 'NONE',  ( -5.588000000000000078, -3544.061999999999898, 2254.250000000000000 ) ) ;
#12821 = CARTESIAN_POINT ( 'NONE',  ( 7.279738514679607420, -3581.306672009827253, 2245.940466658847527 ) ) ;
#12822 = DIRECTION ( 'NONE',  ( 0.000000000000000000, -1.000000000000000000, 0.000000000000000000 ) ) ;
#12823 = AXIS2_PLACEMENT_3D ( 'NONE', #521, #2614, #4266 ) ;
#12824 = COORDINATED_UNIVERSAL_TIME_OFFSET ( 0, 0, .AHEAD. ) ;
#12825 = CARTESIAN_POINT ( 'NONE',  ( 132.0583097651000060, -3544.202533098000458, 2260.545675974999995 ) ) ;
#12826 = ORIENTED_EDGE ( 'NONE', *, *, #2844, .T. ) ;
#12827 = CIRCLE ( 'NONE', #2709, 2.844800000000091700 ) ;
#12828 = ADVANCED_FACE ( 'NONE', ( #10743 ), #18125, .T. ) ;
#12829 = ADVANCED_FACE ( 'NONE', ( #14499 ), #17887, .T. ) ;
#12830 = TOROIDAL_SURFACE ( 'NONE', #13952, 3.606799999999999784, 0.7620000000000000107 ) ;
#12831 = DIRECTION ( 'NONE',  ( 0.000000000000000000, 0.000000000000000000, -1.000000000000000000 ) ) ;
#12832 = DIRECTION ( 'NONE',  ( 0.000000000000000000, -1.000000000000000000, 0.000000000000000000 ) ) ;
#12833 = DIRECTION ( 'NONE',  ( 1.000000000000000000, 0.000000000000000000, 0.000000000000000000 ) ) ;
#12834 = VERTEX_POINT ( 'NONE', #16469 ) ;
#12835 = DIRECTION ( 'NONE',  ( 0.000000000000000000, 1.000000000000000000, 0.000000000000000000 ) ) ;
#12836 = AXIS2_PLACEMENT_3D ( 'NONE', #8265, #11428, #8034 ) ;
#12837 = AXIS2_PLACEMENT_3D ( 'NONE', #5284, #12658, #16058 ) ;
#12838 = FACE_OUTER_BOUND ( 'NONE', #8514, .T. ) ;
#12839 = VERTEX_POINT ( 'NONE', #14843 ) ;
#12840 = LINE ( 'NONE', #10740, #22281 ) ;
#12841 = ORIENTED_EDGE ( 'NONE', *, *, #21850, .T. ) ;
#12842 = CARTESIAN_POINT ( 'NONE',  ( 142.0316867971999955, -3578.148799999999937, 2239.391000000000076 ) ) ;
#12843 = ADVANCED_FACE ( 'NONE', ( #16582 ), #16361, .F. ) ;
#12844 = DIRECTION ( 'NONE',  ( 0.000000000000000000, 0.000000000000000000, 1.000000000000000000 ) ) ;
#12845 = TOROIDAL_SURFACE ( 'NONE', #22524, 5.080000000000000071, 0.3810000000000000053 ) ;
#12846 = AXIS2_PLACEMENT_3D ( 'NONE', #8689, #19006, #4704 ) ;
#12847 = DIRECTION ( 'NONE',  ( 0.9999999999969670927, 2.462891091727920355E-06, 0.000000000000000000 ) ) ;
#12848 = CARTESIAN_POINT ( 'NONE',  ( 142.3391676994775707, -3543.814512434918015, 2255.525709086601182 ) ) ;
#12849 = DIRECTION ( 'NONE',  ( -0.8660254037817187722, 0.5000000000047108983, 0.000000000000000000 ) ) ;
#12850 = CARTESIAN_POINT ( 'NONE',  ( 7.338124605662116551, -3577.517127564773546, 2244.882856471110699 ) ) ;
#12851 = ORIENTED_EDGE ( 'NONE', *, *, #7703, .T. ) ;
#12852 = APPROVAL_ROLE ( '' ) ;
#12853 = CARTESIAN_POINT ( 'NONE',  ( -12.69999999979406091, -3657.265370510263438, 2247.391999999993459 ) ) ;
#12854 = FACE_OUTER_BOUND ( 'NONE', #22576, .T. ) ;
#12856 = AXIS2_PLACEMENT_3D ( 'NONE', #8547, #15690, #18845 ) ;
#12855 = DATE_AND_TIME ( #7468, #9745 ) ;
#12857 = DIRECTION ( 'NONE',  ( -5.461016542361937364E-28, 1.000000000000000000, -2.336881798971000105E-14 ) ) ;
#12858 = VECTOR ( 'NONE', #431, 1000.000000000000000 ) ;
#12859 = CARTESIAN_POINT ( 'NONE',  ( 15.54479999999999862, -3579.494999999999891, 2272.030000000000200 ) ) ;
#12860 = AXIS2_PLACEMENT_3D ( 'NONE', #20152, #4087, #11233 ) ;
#12861 = ORIENTED_EDGE ( 'NONE', *, *, #22453, .F. ) ;
#12862 = CARTESIAN_POINT ( 'NONE',  ( 0.7620000000000000107, -3544.061999999999898, 2295.829799999999977 ) ) ;
#12863 = ADVANCED_FACE ( 'NONE', ( #3587 ), #1834, .T. ) ;
#12864 = TOROIDAL_SURFACE ( 'NONE', #19983, 1.905000000000000027, 1.270000000000000018 ) ;
#12865 = EDGE_CURVE ( 'NONE', #7211, #16324, #19632, .T. ) ;
#12866 = EDGE_CURVE ( 'NONE', #15615, #5409, #12960, .T. ) ;
#12867 = VERTEX_POINT ( 'NONE', #21640 ) ;
#12868 = CARTESIAN_POINT ( 'NONE',  ( 136.8551999999999964, -3579.494999999999891, 2256.063560000000052 ) ) ;
#12869 = ORIENTED_EDGE ( 'NONE', *, *, #19465, .T. ) ;
#12870 = CARTESIAN_POINT ( 'NONE',  ( 11.18976463363000029, -3637.084503524999491, 2279.715692703000059 ) ) ;
#12871 = ORIENTED_EDGE ( 'NONE', *, *, #14939, .F. ) ;
#12872 = ADVANCED_FACE ( 'NONE', ( #78 ), #10644, .T. ) ;
#12873 = CARTESIAN_POINT ( 'NONE',  ( 142.0316867971999955, -3658.158799999999701, 2242.820000000000164 ) ) ;
#12874 = CIRCLE ( 'NONE', #21492, 6.349999999999855760 ) ;
#12875 = ORIENTED_EDGE ( 'NONE', *, *, #3835, .T. ) ;
#12876 = DIRECTION ( 'NONE',  ( 0.000000000000000000, 0.000000000000000000, -1.000000000000000000 ) ) ;
#12877 = DIRECTION ( 'NONE',  ( -2.324635735433000053E-14, 2.336881798971000105E-14, -1.000000000000000000 ) ) ;
#12878 = EDGE_CURVE ( 'NONE', #5052, #6867, #4649, .T. ) ;
#12879 = ORIENTED_EDGE ( 'NONE', *, *, #17396, .F. ) ;
#12880 = EDGE_CURVE ( 'NONE', #22049, #5314, #11685, .T. ) ;
#12881 = CARTESIAN_POINT ( 'NONE',  ( 137.6646844684655662, -3581.483553633650899, 2248.496591272957176 ) ) ;
#12882 = VERTEX_POINT ( 'NONE', #18574 ) ;
#12883 = CARTESIAN_POINT ( 'NONE',  ( 12.69999999999999929, -3599.497499999999945, 2290.241799999999785 ) ) ;
#12884 = APPROVAL_STATUS ( 'not_yet_approved' ) ;
#12885 = CARTESIAN_POINT ( 'NONE',  ( 14.71622237244000075, -3641.518131980000362, 2279.634029254999859 ) ) ;
#12886 = PLANE ( 'NONE',  #14821 ) ;
#12887 = CIRCLE ( 'NONE', #7644, 2.844799999999009010 ) ;
#12888 = CARTESIAN_POINT ( 'NONE',  ( -8.890000000028999594, -3574.821399999999812, 2245.060313203000078 ) ) ;
#12889 = CARTESIAN_POINT ( 'NONE',  ( 9.970475488813999476, -3578.677501247999771, 2257.932973791000222 ) ) ;
#12890 = ADVANCED_FACE ( 'NONE', ( #6282 ), #1094, .F. ) ;
#12891 = CIRCLE ( 'NONE', #20746, 3.606799999998994366 ) ;
#12892 = CARTESIAN_POINT ( 'NONE',  ( 137.9713325200793292, -3577.235569966525418, 2249.727464718754163 ) ) ;
#12893 = ORIENTED_EDGE ( 'NONE', *, *, #12662, .T. ) ;
#12894 = CARTESIAN_POINT ( 'NONE',  ( 134.4866660653693202, -3577.153554363255353, 2245.115832528504598 ) ) ;
#12895 = FACE_OUTER_BOUND ( 'NONE', #18182, .T. ) ;
#12896 = EDGE_LOOP ( 'NONE', ( #17580, #14695, #20874, #17549 ) ) ;
#12897 = CARTESIAN_POINT ( 'NONE',  ( 15.11851230223999920, -3597.988080951000029, 2279.551734718999796 ) ) ;
#12898 = CARTESIAN_POINT ( 'NONE',  ( 139.6999999999999886, -3584.956000000000131, 2239.391000000000076 ) ) ;
#12899 = VERTEX_POINT ( 'NONE', #22308 ) ;
#12900 = CARTESIAN_POINT ( 'NONE',  ( 14.90539642439000012, -3661.309404879999875, 2257.813168336999752 ) ) ;
#12901 = DIRECTION ( 'NONE',  ( 0.8660254037827048723, 0.5000000000030029312, 0.000000000000000000 ) ) ;
#12902 = AXIS2_PLACEMENT_3D ( 'NONE', #15427, #19057, #8397 ) ;
#12903 = ORIENTED_EDGE ( 'NONE', *, *, #16114, .T. ) ;
#12904 = CIRCLE ( 'NONE', #15144, 5.715000000001027480 ) ;
#12905 = FACE_OUTER_BOUND ( 'NONE', #15173, .T. ) ;
#12906 = FACE_OUTER_BOUND ( 'NONE', #18491, .T. ) ;
#12907 = VECTOR ( 'NONE', #18316, 1000.000000000000000 ) ;
#12908 = CARTESIAN_POINT ( 'NONE',  ( 116.8400000000000034, -3568.700000000000273, 2247.392000000000280 ) ) ;
#12909 = ORIENTED_EDGE ( 'NONE', *, *, #17963, .T. ) ;
#12910 = FACE_OUTER_BOUND ( 'NONE', #22932, .T. ) ;
#12911 = APPROVAL_DATE_TIME ( #22038, #5337 ) ;
#12912 = CARTESIAN_POINT ( 'NONE',  ( 12.70000000000085194, -3602.342301254449922, 2279.817638608976267 ) ) ;
#12913 = DIRECTION ( 'NONE',  ( 0.000000000000000000, -1.000000000000000000, 0.000000000000000000 ) ) ;
#12914 = EDGE_LOOP ( 'NONE', ( #9133, #18039, #700, #21923 ) ) ;
#12915 = CARTESIAN_POINT ( 'NONE',  ( 18.17636274929951057, -3581.130155322544852, 2245.675470980243063 ) ) ;
#12916 = CARTESIAN_POINT ( 'NONE',  ( 139.3259398351677874, -3576.668784357255845, 2257.597438745286581 ) ) ;
#12917 = ORIENTED_EDGE ( 'NONE', *, *, #5932, .F. ) ;
#12918 = AXIS2_PLACEMENT_3D ( 'NONE', #14084, #2829, #5184 ) ;
#12919 = ORIENTED_EDGE ( 'NONE', *, *, #9239, .T. ) ;
#12920 = AXIS2_PLACEMENT_3D ( 'NONE', #3808, #18223, #5700 ) ;
#12921 = CARTESIAN_POINT ( 'NONE',  ( 139.1601031653451344, -3662.312941375153969, 2249.232129089474256 ) ) ;
#12922 = APPLIED_PERSON_AND_ORGANIZATION_ASSIGNMENT ( #6464, #2815, ( #7149 ) ) ;
#12923 = AXIS2_PLACEMENT_3D ( 'NONE', #17322, #11474, #22362 ) ;
#12924 = ORIENTED_EDGE ( 'NONE', *, *, #9378, .T. ) ;
#12925 = VERTEX_POINT ( 'NONE', #984 ) ;
#12926 = CARTESIAN_POINT ( 'NONE',  ( 12.69999999999999929, -3654.043999999999869, 2244.978999999999814 ) ) ;
#12927 = EDGE_CURVE ( 'NONE', #22190, #6461, #13415, .T. ) ;
#12928 = VERTEX_POINT ( 'NONE', #7913 ) ;
#12929 = DIRECTION ( 'NONE',  ( 2.324635735433000053E-14, 0.000000000000000000, 1.000000000000000000 ) ) ;
#12930 = ADVANCED_FACE ( 'NONE', ( #16701 ), #20549, .F. ) ;
#12931 = ORIENTED_EDGE ( 'NONE', *, *, #15951, .F. ) ;
#12932 = DIRECTION ( 'NONE',  ( 0.000000000000000000, -1.000000000000000000, 0.000000000000000000 ) ) ;
#12933 = DIRECTION ( 'NONE',  ( -1.000000000000000000, 0.000000000000000000, 0.000000000000000000 ) ) ;
#12934 = AXIS2_PLACEMENT_3D ( 'NONE', #16951, #888, #6311 ) ;
#12935 = AXIS2_PLACEMENT_3D ( 'NONE', #20381, #2679, #9826 ) ;
#12936 = DIRECTION ( 'NONE',  ( 0.000000000000000000, 0.000000000000000000, -1.000000000000000000 ) ) ;
#12937 = PERSON_AND_ORGANIZATION_ROLE ( 'creator' ) ;
#12938 =( REPRESENTATION_RELATIONSHIP ('NONE','NONE', #20448, #9499 ) REPRESENTATION_RELATIONSHIP_WITH_TRANSFORMATION ( #15218 )SHAPE_REPRESENTATION_RELATIONSHIP( ) );
#12939 = CIRCLE ( 'NONE', #5476, 0.3810000000000002829 ) ;
#12940 = DIRECTION ( 'NONE',  ( -1.000000000000000000, 0.000000000000000000, 0.000000000000000000 ) ) ;
#12941 = ORIENTED_EDGE ( 'NONE', *, *, #367, .T. ) ;
#12942 = AXIS2_PLACEMENT_3D ( 'NONE', #4582, #9972, #948 ) ;
#12943 = CARTESIAN_POINT ( 'NONE',  ( 142.5260164572884491, -3659.173939949165742, 2250.068209961469165 ) ) ;
#12944 = CARTESIAN_POINT ( 'NONE',  ( 7.603979357582005605, -3662.088066489251560, 2245.312755012078469 ) ) ;
#12945 = B_SPLINE_CURVE_WITH_KNOTS ( 'NONE', 3,
 ( #2908, #11268, #5782, #17077 ),
 .UNSPECIFIED., .F., .F.,
 ( 4, 4 ),
 ( 0.000000000000000000, 1.000000000000000000 ),
 .UNSPECIFIED. ) ;
#12946 = EDGE_LOOP ( 'NONE', ( #22021, #16382, #20080, #15193 ) ) ;
#12947 = DIRECTION ( 'NONE',  ( -1.000000000000000000, -2.848935406719999894E-12, 0.000000000000000000 ) ) ;
#12948 = PRODUCT_RELATED_PRODUCT_CATEGORY ( 'detail', '', ( #10501 ) ) ;
#12949 = CIRCLE ( 'NONE', #2838, 0.3809999999999993947 ) ;
#12950 = DIRECTION ( 'NONE',  ( 1.000000000000000000, 5.432398939370943590E-28, -2.324635735433000369E-14 ) ) ;
#12951 = DIRECTION ( 'NONE',  ( -0.000000000000000000, 1.000000000000000000, 0.000000000000000000 ) ) ;
#12952 = VECTOR ( 'NONE', #13095, 1000.000000000000000 ) ;
#12953 = DIRECTION ( 'NONE',  ( 0.000000000000000000, 0.000000000000000000, 1.000000000000000000 ) ) ;
#12954 = PRODUCT_DEFINITION_SHAPE ( 'NONE', 'NONE',  #23179 ) ;
#12955 = AXIS2_PLACEMENT_3D ( 'NONE', #14006, #10477, #8732 ) ;
#12956 = CARTESIAN_POINT ( 'NONE',  ( 147.6246907140292706, -3543.405519448600899, 2259.836836426394711 ) ) ;
#12957 = EDGE_CURVE ( 'NONE', #13496, #7929, #15508, .T. ) ;
#12958 = ORIENTED_EDGE ( 'NONE', *, *, #4770, .F. ) ;
#12959 = CARTESIAN_POINT ( 'NONE',  ( 147.6218842717319717, -3695.591362401009519, 2259.843974340487421 ) ) ;
#12960 = LINE ( 'NONE', #16129, #20011 ) ;
#12961 = AXIS2_PLACEMENT_3D ( 'NONE', #10144, #15538, #4519 ) ;
#12962 = EDGE_CURVE ( 'NONE', #13565, #18622, #18504, .T. ) ;
#12963 = DIRECTION ( 'NONE',  ( 0.8660254037821217832, -0.5000000000040129011, 0.000000000000000000 ) ) ;
#12964 = EDGE_CURVE ( 'NONE', #22920, #7890, #4272, .T. ) ;
#12965 = AXIS2_PLACEMENT_3D ( 'NONE', #18819, #2889, #11910 ) ;
#12966 = PLANE ( 'NONE',  #11947 ) ;
#12967 = DIRECTION ( 'NONE',  ( -1.000000000000000000, 0.000000000000000000, 0.000000000000000000 ) ) ;
#12968 = VECTOR ( 'NONE', #10382, 1000.000000000000000 ) ;
#12969 = FACE_OUTER_BOUND ( 'NONE', #7512, .T. ) ;
#12970 = CARTESIAN_POINT ( 'NONE',  ( 6.985000000000999520, -3599.497499999999945, 2295.829799999999977 ) ) ;
#12971 = VERTEX_POINT ( 'NONE', #22193 ) ;
#12972 = APPROVAL_ROLE ( '' ) ;
#12973 = CARTESIAN_POINT ( 'NONE',  ( 145.0128742528000032, -3657.399152860999493, 2246.630000000000109 ) ) ;
#12974 = EDGE_CURVE ( 'NONE', #22532, #894, #12652, .T. ) ;
#12975 = DIRECTION ( 'NONE',  ( 2.236068172604000108E-13, -1.295098308114000000E-13, 1.000000000000000000 ) ) ;
#12976 = PLANE ( 'NONE',  #8690 ) ;
#12977 = DIRECTION ( 'NONE',  ( -1.744774614850039793E-12, -0.5000000000047110094, -0.8660254037817188832 ) ) ;
#12978 = EDGE_CURVE ( 'NONE', #12078, #3416, #4619, .T. ) ;
#12979 = VECTOR ( 'NONE', #19081, 1000.000000000000000 ) ;
#12980 = ORIENTED_EDGE ( 'NONE', *, *, #10113, .T. ) ;
#12981 = AXIS2_PLACEMENT_3D ( 'NONE', #3925, #642, #7335 ) ;
#12982 = DIRECTION ( 'NONE',  ( 0.000000000000000000, 0.000000000000000000, 1.000000000000000000 ) ) ;
#12983 = CIRCLE ( 'NONE', #2870, 0.7619999999999294005 ) ;
#12984 = ORIENTED_EDGE ( 'NONE', *, *, #10137, .T. ) ;
#12985 = DIRECTION ( 'NONE',  ( 1.000000000000000000, 0.000000000000000000, 0.000000000000000000 ) ) ;
#12986 = ORIENTED_EDGE ( 'NONE', *, *, #21752, .F. ) ;
#12987 = CARTESIAN_POINT ( 'NONE',  ( -12.31900000000000084, -3581.209255678999853, 2248.748343399000532 ) ) ;
#12988 = DIRECTION ( 'NONE',  ( 0.000000000000000000, 0.000000000000000000, -1.000000000000000000 ) ) ;
#12989 = ORIENTED_EDGE ( 'NONE', *, *, #17658, .T. ) ;
#12990 = FACE_OUTER_BOUND ( 'NONE', #12946, .T. ) ;
#12991 = AXIS2_PLACEMENT_3D ( 'NONE', #352, #1761, #11133 ) ;
#12992 = DIRECTION ( 'NONE',  ( 0.000000000000000000, 1.000000000000000000, 0.000000000000000000 ) ) ;
#12993 = EDGE_CURVE ( 'NONE', #13145, #8256, #2740, .T. ) ;
#12994 = ORIENTED_EDGE ( 'NONE', *, *, #22441, .F. ) ;
#12995 = DIRECTION ( 'NONE',  ( 0.000000000000000000, 0.000000000000000000, -1.000000000000000000 ) ) ;
#12996 = CARTESIAN_POINT ( 'NONE',  ( 3.810000000000000053, -3544.061999999999898, 2229.612000000000080 ) ) ;
#12997 = PERSON ( 'NAUO-PER7', 'UNSPECIFIED', 'UNSPECIFIED', ('UNSPECIFIED'), ('UNSPECIFIED'), ('UNSPECIFIED') ) ;
#12998 = CIRCLE ( 'NONE', #18242, 4.114799999999974034 ) ;
#12999 = VERTEX_POINT ( 'NONE', #752 ) ;
#13000 = EDGE_CURVE ( 'NONE', #2800, #18918, #16723, .T. ) ;
#13001 = ADVANCED_FACE ( 'NONE', ( #15176 ), #10011, .F. ) ;
#13002 = DIRECTION ( 'NONE',  ( 0.000000000000000000, 0.000000000000000000, -1.000000000000000000 ) ) ;
#13003 = UNCERTAINTY_MEASURE_WITH_UNIT (LENGTH_MEASURE( 1.000000000000000082E-05 ), #16076, 'distance_accuracy_value', 'NONE');
#13004 = VERTEX_POINT ( 'NONE', #8258 ) ;
#13005 = CARTESIAN_POINT ( 'NONE',  ( 145.3885918142797777, -3580.043763408794803, 2244.804994013378746 ) ) ;
#13006 = PERSON_AND_ORGANIZATION ( #5446, #1895 ) ;
#13007 = CARTESIAN_POINT ( 'NONE',  ( 12.69999999999999929, -3656.329999999999472, 2270.760000000000218 ) ) ;
#13008 = DIRECTION ( 'NONE',  ( 0.000000000000000000, -1.000000000000000000, 0.000000000000000000 ) ) ;
#13009 = ADVANCED_FACE ( 'NONE', ( #21974 ), #5940, .T. ) ;
#13010 = CYLINDRICAL_SURFACE ( 'NONE', #19350, 0.3809999999999924558 ) ;
#13011 = CARTESIAN_POINT ( 'NONE',  ( 139.6999999999999886, -3574.034000000000106, 2244.978999999999814 ) ) ;
#13012 = CIRCLE ( 'NONE', #16369, 5.080000000000000071 ) ;
#13013 = CARTESIAN_POINT ( 'NONE',  ( 141.9354122741817150, -3577.734584490984162, 2250.005152421867933 ) ) ;
#13014 = ORIENTED_EDGE ( 'NONE', *, *, #13164, .T. ) ;
#13015 = ADVANCED_FACE ( 'NONE', ( #11307 ), #18458, .F. ) ;
#13016 = AXIS2_PLACEMENT_3D ( 'NONE', #14861, #9685, #2315 ) ;
#13017 = VECTOR ( 'NONE', #16313, 1000.000000000000000 ) ;
#13018 = DIRECTION ( 'NONE',  ( 0.000000000000000000, 0.000000000000000000, 1.000000000000000000 ) ) ;
#13019 = ORIENTED_EDGE ( 'NONE', *, *, #12245, .T. ) ;
#13020 = FACE_OUTER_BOUND ( 'NONE', #1687, .T. ) ;
#13021 = CARTESIAN_POINT ( 'NONE',  ( 142.1839422283480872, -3660.940228195818236, 2257.872821505005959 ) ) ;
#13022 = ORIENTED_EDGE ( 'NONE', *, *, #740, .F. ) ;
#13023 = AXIS2_PLACEMENT_3D ( 'NONE', #16448, #19980, #16342 ) ;
#13024 = LINE ( 'NONE', #10416, #2678 ) ;
#13025 = CARTESIAN_POINT ( 'NONE',  ( 12.69999999999999929, -3577.590000000000146, 2270.760000000000218 ) ) ;
#13026 = EDGE_LOOP ( 'NONE', ( #1889, #11436, #5159, #18695 ) ) ;
#13027 = VECTOR ( 'NONE', #16743, 1000.000000000000000 ) ;
#13028 = ADVANCED_FACE ( 'NONE', ( #1449 ), #5214, .T. ) ;
#13029 = CARTESIAN_POINT ( 'NONE',  ( 14.48098936461540553, -3577.276529815265349, 2249.755429883363831 ) ) ;
#13030 = SHAPE_REPRESENTATION_RELATIONSHIP ( 'NONE' , 'NONE' ,  #536, #9899 ) ;
#13031 = CARTESIAN_POINT ( 'NONE',  ( 147.3199999999999932, -3695.699999999999818, 2260.600000000000364 ) ) ;
#13032 = VERTEX_POINT ( 'NONE', #21151 ) ;
#13033 = CARTESIAN_POINT ( 'NONE',  ( 95.25000000000000000, -3544.570000000000164, 2247.392000000000280 ) ) ;
#13034 = PERSON_AND_ORGANIZATION ( #5446, #1895 ) ;
#13035 = CIRCLE ( 'NONE', #2917, 0.3809999999999647002 ) ;
#13036 = CARTESIAN_POINT ( 'NONE',  ( 9.855200508358999301, -3659.504990670146526, 2257.962940201000038 ) ) ;
#13037 = DIRECTION ( 'NONE',  ( 0.000000000000000000, 0.000000000000000000, -1.000000000000000000 ) ) ;
#13038 = DIRECTION ( 'NONE',  ( -1.000000000000000000, 0.000000000000000000, 0.000000000000000000 ) ) ;
#13039 = CARTESIAN_POINT ( 'NONE',  ( 136.9337416949390729, -3658.818840990081753, 2249.918292882339756 ) ) ;
#13040 = ORIENTED_EDGE ( 'NONE', *, *, #2901, .F. ) ;
#13041 = CARTESIAN_POINT ( 'NONE',  ( 141.3692361696618320, -3661.808694985247257, 2249.696048052667720 ) ) ;
#13042 = EDGE_CURVE ( 'NONE', #22793, #3779, #3922, .T. ) ;
#13043 = VECTOR ( 'NONE', #5662, 1000.000000000000000 ) ;
#13044 = ORIENTED_EDGE ( 'NONE', *, *, #12510, .F. ) ;
#13045 = VERTEX_POINT ( 'NONE', #22770 ) ;
#13046 = DIRECTION ( 'NONE',  ( 1.000000000000000000, -1.165588477296748772E-12, 0.000000000000000000 ) ) ;
#13047 = ORIENTED_EDGE ( 'NONE', *, *, #8678, .T. ) ;
#13048 = DIRECTION ( 'NONE',  ( 0.000000000000000000, -1.000000000000000000, 0.000000000000000000 ) ) ;
#13049 = DATE_AND_TIME ( #17502, #6789 ) ;
#13050 = CARTESIAN_POINT ( 'NONE',  ( 12.69999999999999929, -3594.036500000000160, 2296.210799999999836 ) ) ;
#13051 = VERTEX_POINT ( 'NONE', #8727 ) ;
#13052 = CARTESIAN_POINT ( 'NONE',  ( 7.091956865061221471, -3658.404132852121620, 2245.137126576677019 ) ) ;
#13053 = CARTESIAN_POINT ( 'NONE',  ( 101.5999999999999943, -3670.300000000000182, 2259.837999999999738 ) ) ;
#13054 = LINE ( 'NONE', #20203, #1609 ) ;
#13055 = CARTESIAN_POINT ( 'NONE',  ( 129.8447999999989975, -3619.500000000000000, 2239.771999999999935 ) ) ;
#13056 = PERSON_AND_ORGANIZATION ( #5446, #1895 ) ;
#13057 = APPLIED_DATE_AND_TIME_ASSIGNMENT ( #22348, #2668, ( #16481 ) ) ;
#13058 = FACE_OUTER_BOUND ( 'NONE', #13740, .T. ) ;
#13059 = ORIENTED_EDGE ( 'NONE', *, *, #15440, .F. ) ;
#13060 = CIRCLE ( 'NONE', #10050, 2.844799999998995244 ) ;
#13061 = DIRECTION ( 'NONE',  ( 0.000000000000000000, 1.000000000000000000, 0.000000000000000000 ) ) ;
#13062 = ORIENTED_EDGE ( 'NONE', *, *, #4521, .F. ) ;
#13063 = CARTESIAN_POINT ( 'NONE',  ( 130.6067999999989979, -3670.300000000000182, 2239.771999999999935 ) ) ;
#13064 = ORIENTED_EDGE ( 'NONE', *, *, #6012, .T. ) ;
#13065 = CYLINDRICAL_SURFACE ( 'NONE', #22309, 2.844800000000091700 ) ;
#13066 = DIRECTION ( 'NONE',  ( 1.000000000000000000, 0.000000000000000000, 3.996303350731721563E-14 ) ) ;
#13067 = DIRECTION ( 'NONE',  ( 0.000000000000000000, -1.000000000000000000, 0.000000000000000000 ) ) ;
#13068 = DIRECTION ( 'NONE',  ( 1.206643234470999950E-12, -1.000000000000000000, -2.336881798973999985E-14 ) ) ;
#13069 = ORIENTED_EDGE ( 'NONE', *, *, #10260, .F. ) ;
#13070 = CARTESIAN_POINT ( 'NONE',  ( 147.5857674342917960, -3695.547111920908719, 2259.934514517091884 ) ) ;
#13071 = DIRECTION ( 'NONE',  ( 0.000000000000000000, 0.000000000000000000, -1.000000000000000000 ) ) ;
#13072 = CARTESIAN_POINT ( 'NONE',  ( 127.0000000000000000, -3670.300000000000182, 2239.009999999999764 ) ) ;
#13073 = DIRECTION ( 'NONE',  ( 0.000000000000000000, -1.000000000000000000, 0.000000000000000000 ) ) ;
#13074 = CARTESIAN_POINT ( 'NONE',  ( 142.7013568988404018, -3543.300000000001091, 2254.618513959080701 ) ) ;
#13075 = DIRECTION ( 'NONE',  ( -2.324635735433000053E-14, 2.336881798971000105E-14, -1.000000000000000000 ) ) ;
#13076 = CARTESIAN_POINT ( 'NONE',  ( 7.152845350294700033, -3578.119350159317491, 2244.644855890406689 ) ) ;
#13077 = ORIENTED_EDGE ( 'NONE', *, *, #4779, .F. ) ;
#13078 = PERSON_AND_ORGANIZATION ( #5446, #1895 ) ;
#13079 = APPLIED_PERSON_AND_ORGANIZATION_ASSIGNMENT ( #15851, #12450, ( #19460 ) ) ;
#13080 = CARTESIAN_POINT ( 'NONE',  ( 7.619999999999999218, -3659.504999999999654, 2239.009999999999764 ) ) ;
#13081 = CIRCLE ( 'NONE', #22042, 3.606800000000021100 ) ;
#13082 = CARTESIAN_POINT ( 'NONE',  ( 57.14999999999999858, -3544.570000000000164, 2247.392000000000280 ) ) ;
#13083 = EDGE_CURVE ( 'NONE', #20229, #2094, #23001, .T. ) ;
#13084 = DIRECTION ( 'NONE',  ( 1.000000000000000000, 1.206643234470999950E-12, 0.000000000000000000 ) ) ;
#13085 = APPLIED_APPROVAL_ASSIGNMENT ( #11350, ( #16085 ) ) ;
#13086 = EDGE_CURVE ( 'NONE', #22481, #12839, #17503, .T. ) ;
#13087 = CIRCLE ( 'NONE', #2977, 2.844800000000091700 ) ;
#13088 = ORIENTED_EDGE ( 'NONE', *, *, #12436, .T. ) ;
#13089 = CARTESIAN_POINT ( 'NONE',  ( 134.8457231033459038, -3662.521201777085935, 2245.835328354021385 ) ) ;
#13090 = EDGE_CURVE ( 'NONE', #19652, #12370, #5047, .T. ) ;
#13091 = VERTEX_POINT ( 'NONE', #1212 ) ;
#13092 = CARTESIAN_POINT ( 'NONE',  ( 12.70000000002683471, -3656.630370510377816, 2239.010000000078435 ) ) ;
#13093 = ORIENTED_EDGE ( 'NONE', *, *, #20045, .F. ) ;
#13094 = LINE ( 'NONE', #15086, #14768 ) ;
#13095 = DIRECTION ( 'NONE',  ( 0.000000000000000000, 0.000000000000000000, -1.000000000000000000 ) ) ;
#13096 = ORIENTED_EDGE ( 'NONE', *, *, #2824, .T. ) ;
#13097 = ADVANCED_FACE ( 'NONE', ( #17619 ), #6741, .F. ) ;
#13098 = PLANE ( 'NONE',  #10677 ) ;
#13099 = DIRECTION ( 'NONE',  ( 0.000000000000000000, 1.000000000000000000, 0.000000000000000000 ) ) ;
#13100 = CIRCLE ( 'NONE', #19070, 3.606799999998994366 ) ;
#13101 = EDGE_LOOP ( 'NONE', ( #9216, #8487, #9741, #7372, #6386, #5850 ) ) ;
#13102 = CARTESIAN_POINT ( 'NONE',  ( 12.69999999999999929, -3639.502500000000055, 2290.241799999999785 ) ) ;
#13103 = DIRECTION ( 'NONE',  ( 0.000000000000000000, 0.000000000000000000, -1.000000000000000000 ) ) ;
#13104 = APPLIED_APPROVAL_ASSIGNMENT ( #22502, ( #11230 ) ) ;
#13105 = VERTEX_POINT ( 'NONE', #10240 ) ;
#13106 = AXIS2_PLACEMENT_3D ( 'NONE', #2810, #15593, #18989 ) ;
#13107 = EDGE_LOOP ( 'NONE', ( #15803, #5948, #346, #16823 ) ) ;
#13108 = DIRECTION ( 'NONE',  ( -1.000000000000000000, 0.000000000000000000, 0.000000000000000000 ) ) ;
#13109 = ORIENTED_EDGE ( 'NONE', *, *, #2541, .T. ) ;
#13110 = FACE_OUTER_BOUND ( 'NONE', #10493, .T. ) ;
#13111 = SECURITY_CLASSIFICATION_LEVEL ( 'unclassified' ) ;
#13112 = CARTESIAN_POINT ( 'NONE',  ( 50.79999999999999716, -3619.500000000000000, 2260.600000000000364 ) ) ;
#13113 = CARTESIAN_POINT ( 'NONE',  ( 17.81852837919641175, -3662.046892928622128, 2245.280258281285114 ) ) ;
#13114 = CIRCLE ( 'NONE', #15359, 2.844800000000091700 ) ;
#13115 = CARTESIAN_POINT ( 'NONE',  ( 132.0286848278999798, -3544.241664856000170, 2260.557504477000293 ) ) ;
#13116 = EDGE_CURVE ( 'NONE', #7066, #7706, #10595, .T. ) ;
#13117 = CARTESIAN_POINT ( 'NONE',  ( 10.36831320282916202, -3640.848700000148256, 2296.433984632680676 ) ) ;
#13118 = SECURITY_CLASSIFICATION ( '', '', #13111 ) ;
#13119 = CARTESIAN_POINT ( 'NONE',  ( 141.3710085595040198, -3577.190797867237961, 2249.696701696144373 ) ) ;
#13120 = ORIENTED_EDGE ( 'NONE', *, *, #628, .F. ) ;
#13121 = PRODUCT_DEFINITION_FORMATION_WITH_SPECIFIED_SOURCE ( 'ANY', '', #10108, .NOT_KNOWN. ) ;
#13122 = LINE ( 'NONE', #4103, #5809 ) ;
#13123 = VERTEX_POINT ( 'NONE', #22883 ) ;
#13124 = DIRECTION ( 'NONE',  ( -1.000000000000000000, 0.000000000000000000, 0.000000000000000000 ) ) ;
#13125 = CARTESIAN_POINT ( 'NONE',  ( 140.6195432093131501, -3662.203521821452341, 2257.629402108538216 ) ) ;
#13126 = ORIENTED_EDGE ( 'NONE', *, *, #5118, .F. ) ;
#13127 = VERTEX_POINT ( 'NONE', #19500 ) ;
#13128 = CARTESIAN_POINT ( 'NONE',  ( 0.7620000000000000107, -3544.061999999999898, 2275.001800000000003 ) ) ;
#13129 = ORIENTED_EDGE ( 'NONE', *, *, #22996, .F. ) ;
#13130 = DIRECTION ( 'NONE',  ( -1.000000000000000000, 0.000000000000000000, 0.000000000000000000 ) ) ;
#13131 = CARTESIAN_POINT ( 'NONE',  ( 15.31109373216002645, -3578.363233960815251, 2250.193977524520051 ) ) ;
#13132 = ORGANIZATION ( 'NAUO-ORG6', 'UNSPECIFIED', 'UNSPECIFIED' ) ;
#13133 = CARTESIAN_POINT ( 'NONE',  ( 141.5105608045840881, -3581.689302659061013, 2247.699634051008616 ) ) ;
#13134 = VERTEX_POINT ( 'NONE', #10358 ) ;
#13135 = SECURITY_CLASSIFICATION ( '', '', #7440 ) ;
#13136 = DIRECTION ( 'NONE',  ( 0.000000000000000000, 0.000000000000000000, -1.000000000000000000 ) ) ;
#13137 = PERSON_AND_ORGANIZATION ( #5446, #1895 ) ;
#13138 = DIRECTION ( 'NONE',  ( 0.000000000000000000, 1.000000000000000000, 0.000000000000000000 ) ) ;
#13139 = DIRECTION ( 'NONE',  ( -0.8660254037824819395, -0.5000000000033889558, 5.608020032299880803E-12 ) ) ;
#13140 = ORIENTED_EDGE ( 'NONE', *, *, #896, .T. ) ;
#13141 = CARTESIAN_POINT ( 'NONE',  ( 20.68901695980001421, -3543.347945942427032, 2259.675964649152775 ) ) ;
#13142 = CIRCLE ( 'NONE', #6426, 2.844799999999009010 ) ;
#13143 = CARTESIAN_POINT ( 'NONE',  ( 17.31138602735000021, -3576.119152860999748, 2246.630000000000109 ) ) ;
#13144 = AXIS2_PLACEMENT_3D ( 'NONE', #21377, #15515, #6857 ) ;
#13145 = VERTEX_POINT ( 'NONE', #4739 ) ;
#13146 = CARTESIAN_POINT ( 'NONE',  ( 141.9481709719357525, -3661.250240185189796, 2250.012217711370795 ) ) ;
#13147 = EDGE_CURVE ( 'NONE', #257, #16631, #15906, .T. ) ;
#13148 = EDGE_CURVE ( 'NONE', #22010, #3639, #3161, .T. ) ;
#13149 = EDGE_LOOP ( 'NONE', ( #21277, #7417, #2389, #14874 ) ) ;
#13150 = ADVANCED_FACE ( 'NONE', ( #12117 ), #19265, .T. ) ;
#13151 = EDGE_LOOP ( 'NONE', ( #12276, #23164 ) ) ;
#13152 = CARTESIAN_POINT ( 'NONE',  ( 57.14999999999999858, -3544.570000000000164, 2247.392000000000280 ) ) ;
#13153 = ORIENTED_EDGE ( 'NONE', *, *, #8874, .T. ) ;
#13154 = CARTESIAN_POINT ( 'NONE',  ( 88.90000000000000568, -3594.099999999999909, 2260.600000000000364 ) ) ;
#13155 = CYLINDRICAL_SURFACE ( 'NONE', #1699, 2.844799999998995244 ) ;
#13156 = EDGE_CURVE ( 'NONE', #21069, #20114, #19272, .T. ) ;
#13157 = CIRCLE ( 'NONE', #3048, 2.844800000000091700 ) ;
#13158 = ORIENTED_EDGE ( 'NONE', *, *, #2787, .T. ) ;
#13159 = CARTESIAN_POINT ( 'NONE',  ( 7.023553847508563486, -3658.842518250462035, 2244.860302287378090 ) ) ;
#13160 = CYLINDRICAL_SURFACE ( 'NONE', #1239, 6.349999999999855760 ) ;
#13161 = DIRECTION ( 'NONE',  ( 0.8660254037820785955, -0.5000000000040877302, -3.181634500919918361E-14 ) ) ;
#13162 = EDGE_CURVE ( 'NONE', #1593, #7425, #3208, .T. ) ;
#13163 = DATE_AND_TIME ( #19981, #410 ) ;
#13164 = EDGE_CURVE ( 'NONE', #13920, #6851, #4294, .T. ) ;
#13165 = DIRECTION ( 'NONE',  ( 0.000000000000000000, 0.000000000000000000, 1.000000000000000000 ) ) ;
#13166 = EDGE_LOOP ( 'NONE', ( #14901, #4490, #14875, #1084, #2945 ) ) ;
#13167 = CARTESIAN_POINT ( 'NONE',  ( 12.69999999999999929, -3639.502500000000055, 2263.571799999999712 ) ) ;
#13168 = CARTESIAN_POINT ( 'NONE',  ( -0.7620000000000000107, -3543.299999999999727, 2253.487999999999829 ) ) ;
#13169 = EDGE_LOOP ( 'NONE', ( #6360, #21784, #6020, #16774, #4331 ) ) ;
#13170 = CARTESIAN_POINT ( 'NONE',  ( 137.1599999999999966, -3695.699999999999818, 2255.774000000000342 ) ) ;
#13171 = AXIS2_PLACEMENT_3D ( 'NONE', #8902, #340, #14408 ) ;
#13172 = DIRECTION ( 'NONE',  ( -1.000000000000000000, 5.461016542361937364E-28, 2.336881798970999789E-14 ) ) ;
#13173 = ORIENTED_EDGE ( 'NONE', *, *, #13148, .T. ) ;
#13174 = CARTESIAN_POINT ( 'NONE',  ( -8.890000000047999507, -3577.513800000000174, 2245.060313203000078 ) ) ;
#13175 = ORIENTED_EDGE ( 'NONE', *, *, #10495, .T. ) ;
#13176 = CYLINDRICAL_SURFACE ( 'NONE', #20390, 2.844800000000001550 ) ;
#13177 = ORIENTED_EDGE ( 'NONE', *, *, #10690, .F. ) ;
#13178 = ORIENTED_EDGE ( 'NONE', *, *, #19102, .F. ) ;
#13179 = PLANE ( 'NONE',  #57 ) ;
#13180 = CARTESIAN_POINT ( 'NONE',  ( 20.34169023495000062, -3694.797466901999996, 2260.545675974999995 ) ) ;
#13181 = VECTOR ( 'NONE', #18810, 1000.000000000000000 ) ;
#13182 = CARTESIAN_POINT ( 'NONE',  ( 142.5447999999989861, -3579.494999999999891, 2257.962944264955695 ) ) ;
#13183 = CARTESIAN_POINT ( 'NONE',  ( 25.39999999999999858, -3568.700000000000273, 2259.837999999999738 ) ) ;
#13184 = LINE ( 'NONE', #20454, #1220 ) ;
#13185 = CARTESIAN_POINT ( 'NONE',  ( 151.1299999999999955, -3660.140000000000327, 2247.392000000000280 ) ) ;
#13186 = VECTOR ( 'NONE', #5016, 1000.000000000000114 ) ;
#13187 = DIRECTION ( 'NONE',  ( 2.339144844575037611E-14, 0.000000000000000000, 1.000000000000000000 ) ) ;
#13188 = VERTEX_POINT ( 'NONE', #8496 ) ;
#13189 = DATE_AND_TIME ( #14735, #9748 ) ;
#13190 = AXIS2_PLACEMENT_3D ( 'NONE', #19797, #20032, #3967 ) ;
#13191 = LINE ( 'NONE', #9896, #19517 ) ;
#13192 = LINE ( 'NONE', #20237, #20648 ) ;
#13193 = DIRECTION ( 'NONE',  ( -3.479240369245040749E-14, -0.5000000000042060799, -0.8660254037820102058 ) ) ;
#13194 = EDGE_LOOP ( 'NONE', ( #12893, #21773 ) ) ;
#13195 = TOROIDAL_SURFACE ( 'NONE', #22907, 3.606799999999999784, 0.7620000000000000107 ) ;
#13196 = CARTESIAN_POINT ( 'NONE',  ( 135.0886139726000010, -3662.880847139000252, 2246.630000000000109 ) ) ;
#13197 = DIRECTION ( 'NONE',  ( 0.000000000000000000, 0.000000000000000000, 1.000000000000000000 ) ) ;
#13198 = ORIENTED_EDGE ( 'NONE', *, *, #8303, .T. ) ;
#13199 = CIRCLE ( 'NONE', #4226, 1.269999999999882334 ) ;
#13200 = LINE ( 'NONE', #9689, #7006 ) ;
#13201 = CARTESIAN_POINT ( 'NONE',  ( 14.84616252414837945, -3661.372340446721864, 2249.956039958307429 ) ) ;
#13202 = APPLIED_DATE_AND_TIME_ASSIGNMENT ( #5, #10776, ( #5262 ) ) ;
#13203 = AXIS2_PLACEMENT_3D ( 'NONE', #13303, #5833, #4169 ) ;
#13204 = DIRECTION ( 'NONE',  ( 0.000000000000000000, 1.000000000000000000, 0.000000000000000000 ) ) ;
#13205 = VERTEX_POINT ( 'NONE', #15642 ) ;
#13206 = CARTESIAN_POINT ( 'NONE',  ( 25.39999999999999858, -3568.700000000000273, 2239.771999999999935 ) ) ;
#13207 = DIRECTION ( 'NONE',  ( 2.339144844575037611E-14, 0.000000000000000000, 1.000000000000000000 ) ) ;
#13208 = EDGE_CURVE ( 'NONE', #19866, #6944, #22993, .T. ) ;
#13209 = DIRECTION ( 'NONE',  ( 1.000000000000000000, -2.334777064353000131E-14, -2.343004830739999973E-14 ) ) ;
#13210 = DIRECTION ( 'NONE',  ( 1.000000000000000000, 0.000000000000000000, 0.000000000000000000 ) ) ;
#13211 = EDGE_CURVE ( 'NONE', #3211, #724, #15146, .T. ) ;
#13212 = EDGE_LOOP ( 'NONE', ( #13230, #17747, #15350, #20392 ) ) ;
#13213 = VECTOR ( 'NONE', #5402, 1000.000000000000000 ) ;
#13214 = ORIENTED_EDGE ( 'NONE', *, *, #10239, .F. ) ;
#13215 = EDGE_CURVE ( 'NONE', #4556, #1232, #11773, .T. ) ;
#13216 = CYLINDRICAL_SURFACE ( 'NONE', #1955, 0.3809999999998149867 ) ;
#13217 = UNCERTAINTY_MEASURE_WITH_UNIT (LENGTH_MEASURE( 1.000000000000000082E-05 ), #18066, 'distance_accuracy_value', 'NONE');
#13218 = ORIENTED_EDGE ( 'NONE', *, *, #3717, .F. ) ;
#13220 = DIRECTION ( 'NONE',  ( 0.000000000000000000, 0.000000000000000000, 1.000000000000000000 ) ) ;
#13219 = VECTOR ( 'NONE', #10832, 1000.000000000000114 ) ;
#13221 = PERSON_AND_ORGANIZATION ( #5446, #1895 ) ;
#13222 = FACE_OUTER_BOUND ( 'NONE', #18328, .T. ) ;
#13223 = CARTESIAN_POINT ( 'NONE',  ( 17.91765463811091763, -3661.836797945709804, 2245.108621132138069 ) ) ;
#13224 = DIRECTION ( 'NONE',  ( 0.000000000000000000, 0.000000000000000000, -1.000000000000000000 ) ) ;
#13225 = CARTESIAN_POINT ( 'NONE',  ( 72.59320000000001016, -3568.700000000000273, 2259.837999999999738 ) ) ;
#13226 = LINE ( 'NONE', #18972, #13247 ) ;
#13227 = ORIENTED_EDGE ( 'NONE', *, *, #4197, .T. ) ;
#13228 = AXIS2_PLACEMENT_3D ( 'NONE', #15648, #17040, #2745 ) ;
#13229 = DIRECTION ( 'NONE',  ( 0.000000000000000000, 0.000000000000000000, 1.000000000000000000 ) ) ;
#13230 = ORIENTED_EDGE ( 'NONE', *, *, #9066, .F. ) ;
#13231 = LINE ( 'NONE', #11698, #5829 ) ;
#13232 = CARTESIAN_POINT ( 'NONE',  ( 15.66193311550068046, -3543.315017895616620, 2254.716481486307202 ) ) ;
#13233 = ORIENTED_EDGE ( 'NONE', *, *, #2541, .F. ) ;
#13234 = VERTEX_POINT ( 'NONE', #21840 ) ;
#13235 = EDGE_CURVE ( 'NONE', #22306, #16307, #18204, .T. ) ;
#13236 = ORIENTED_EDGE ( 'NONE', *, *, #5455, .F. ) ;
#13237 = CARTESIAN_POINT ( 'NONE',  ( 139.6999999999999886, -3654.043999999999869, 2244.978999999999814 ) ) ;
#13238 = ADVANCED_FACE ( 'NONE', ( #8957 ), #1808, .T. ) ;
#13239 = EDGE_CURVE ( 'NONE', #572, #16435, #2791, .T. ) ;
#13240 = EDGE_LOOP ( 'NONE', ( #22068, #1577, #20585, #6870 ) ) ;
#13241 = ADVANCED_FACE ( 'NONE', ( #17973 ), #561, .T. ) ;
#13242 = DIRECTION ( 'NONE',  ( -1.000000000000000000, 0.000000000000000000, 0.000000000000000000 ) ) ;
#13243 = CARTESIAN_POINT ( 'NONE',  ( 15.04722453113185132, -3577.885471855124251, 2250.065661091934544 ) ) ;
#13244 = CARTESIAN_POINT ( 'NONE',  ( 141.7948968975624950, -3581.419701962929139, 2248.633431646152076 ) ) ;
#13245 = ORIENTED_EDGE ( 'NONE', *, *, #20468, .F. ) ;
#13246 = CARTESIAN_POINT ( 'NONE',  ( 151.1299999999999955, -3695.699999999999818, 2240.279999999999745 ) ) ;
#13247 = VECTOR ( 'NONE', #20377, 1000.000000000000000 ) ;
#13248 = PERSON_AND_ORGANIZATION ( #5446, #1895 ) ;
#13249 = AXIS2_PLACEMENT_3D ( 'NONE', #5128, #14262, #12270 ) ;
#13250 = FACE_OUTER_BOUND ( 'NONE', #3751, .T. ) ;
#13251 = CARTESIAN_POINT ( 'NONE',  ( 20.34169023495000062, -3544.202533098000458, 2260.545675974999995 ) ) ;
#13252 = CARTESIAN_POINT ( 'NONE',  ( 137.9648832672151570, -3577.232990426899960, 2257.727830858807920 ) ) ;
#13253 = ADVANCED_FACE ( 'NONE', ( #14697 ), #17769, .T. ) ;
#13254 = ORIENTED_EDGE ( 'NONE', *, *, #17458, .F. ) ;
#13255 = SHAPE_REPRESENTATION ( 'Hinge 2', ( #5611 ), #1485 ) ;
#13256 = CARTESIAN_POINT ( 'NONE',  ( -12.31900000000000084, -3577.513799999878302, 2245.060313203211081 ) ) ;
#13257 = ORIENTED_EDGE ( 'NONE', *, *, #17070, .F. ) ;
#13258 = ORIENTED_EDGE ( 'NONE', *, *, #10577, .F. ) ;
#13259 = AXIS2_PLACEMENT_3D ( 'NONE', #224, #5381, #9003 ) ;
#13260 = CIRCLE ( 'NONE', #22608, 2.844800000000001550 ) ;
#13261 = CYLINDRICAL_SURFACE ( 'NONE', #15159, 0.3810000000000011156 ) ;
#13262 = AXIS2_PLACEMENT_3D ( 'NONE', #12001, #2976, #6977 ) ;
#13263 = VERTEX_POINT ( 'NONE', #10939 ) ;
#13264 = ORIENTED_EDGE ( 'NONE', *, *, #9304, .T. ) ;
#13265 = CARTESIAN_POINT ( 'NONE',  ( 139.6999999999999886, -3664.965999999999894, 2239.391000000000076 ) ) ;
#13266 = DIRECTION ( 'NONE',  ( 1.000000000000000000, 0.000000000000000000, 0.000000000000000000 ) ) ;
#13267 = ORIENTED_EDGE ( 'NONE', *, *, #10943, .F. ) ;
#13268 = ADVANCED_FACE ( 'NONE', ( #14581 ), #20089, .F. ) ;
#13269 = CARTESIAN_POINT ( 'NONE',  ( 7.011289150263468883, -3658.957678416667932, 2244.804336643922852 ) ) ;
#13270 = FACE_OUTER_BOUND ( 'NONE', #20020, .T. ) ;
#13271 = PERSON ( 'NAUO-PER9', 'UNSPECIFIED', 'UNSPECIFIED', ('UNSPECIFIED'), ('UNSPECIFIED'), ('UNSPECIFIED') ) ;
#13272 = CARTESIAN_POINT ( 'NONE',  ( 12.69999999999999929, -3656.660200000000259, 2257.592639999999847 ) ) ;
#13273 = PERSON_AND_ORGANIZATION ( #5446, #1895 ) ;
#13274 = EDGE_CURVE ( 'NONE', #12304, #19181, #21724, .T. ) ;
#13275 = EDGE_CURVE ( 'NONE', #7984, #473, #7200, .T. ) ;
#13276 = CARTESIAN_POINT ( 'NONE',  ( 73.35520000000001062, -3670.300000000000182, 2239.771999999999935 ) ) ;
#13277 = AXIS2_PLACEMENT_3D ( 'NONE', #16123, #14491, #21858 ) ;
#13278 = CIRCLE ( 'NONE', #8425, 1.904999999999823501 ) ;
#13279 = DIRECTION ( 'NONE',  ( 2.330758767201999921E-14, 1.000000000000000000, -5.460979050843892707E-28 ) ) ;
#13280 = CARTESIAN_POINT ( 'NONE',  ( 12.69999999999999929, -3585.210000000000036, 2268.705139999999574 ) ) ;
#13281 = AXIS2_PLACEMENT_3D ( 'NONE', #11860, #1304, #20888 ) ;
#13282 = EDGE_CURVE ( 'NONE', #22793, #6119, #53, .T. ) ;
#13283 = ORIENTED_EDGE ( 'NONE', *, *, #10986, .T. ) ;
#13284 = DIRECTION ( 'NONE',  ( 0.000000000000000000, 0.000000000000000000, 1.000000000000000000 ) ) ;
#13285 = MANIFOLD_SOLID_BREP ( 'SOLID45-11[1]', #16962 ) ;
#13286 = CYLINDRICAL_SURFACE ( 'NONE', #14045, 5.460999999999938126 ) ;
#13287 = ORIENTED_EDGE ( 'NONE', *, *, #18867, .T. ) ;
#13288 = EDGE_CURVE ( 'NONE', #17042, #18533, #14352, .T. ) ;
#13289 = LINE ( 'NONE', #11412, #1286 ) ;
#13290 = EDGE_CURVE ( 'NONE', #6658, #15415, #15048, .T. ) ;
#13291 = CARTESIAN_POINT ( 'NONE',  ( 18.26100162526913806, -3658.187271764459638, 2245.323245018173566 ) ) ;
#13292 = EDGE_LOOP ( 'NONE', ( #327, #9892, #17876, #16302 ) ) ;
#13293 = EDGE_LOOP ( 'NONE', ( #10763, #4068, #14535, #8693 ) ) ;
#13294 = DIRECTION ( 'NONE',  ( 0.000000000000000000, 1.000000000000000000, 0.000000000000000000 ) ) ;
#13295 = AXIS2_PLACEMENT_3D ( 'NONE', #15145, #2711, #22272 ) ;
#13296 = CARTESIAN_POINT ( 'NONE',  ( 127.0000000000000000, -3670.300000000000182, 2239.771999999999935 ) ) ;
#13297 = VECTOR ( 'NONE', #22134, 1000.000000000000000 ) ;
#13298 = DIRECTION ( 'NONE',  ( -1.000000000000000000, 0.000000000000000000, 0.000000000000000000 ) ) ;
#13299 = VECTOR ( 'NONE', #6420, 1000.000000000000000 ) ;
#13300 = FACE_OUTER_BOUND ( 'NONE', #8493, .T. ) ;
#13301 = AXIS2_PLACEMENT_3D ( 'NONE', #1857, #18362, #557 ) ;
#13302 = DIRECTION ( 'NONE',  ( -2.301834883556000307E-13, -1.295098308109999907E-13, 1.000000000000000000 ) ) ;
#13303 = CARTESIAN_POINT ( 'NONE',  ( 15.03168679717000167, -3580.841199999999844, 2242.820000000000164 ) ) ;
#13304 = CYLINDRICAL_SURFACE ( 'NONE', #12836, 1.269999999999882334 ) ;
#13305 = AXIS2_PLACEMENT_3D ( 'NONE', #9633, #16886, #16775 ) ;
#13306 = ORIENTED_EDGE ( 'NONE', *, *, #2691, .T. ) ;
#13307 = SHAPE_DEFINITION_REPRESENTATION ( #1714, #5332 ) ;
#13308 = ADVANCED_FACE ( 'NONE', ( #17858 ), #1920, .T. ) ;
#13309 = VERTEX_POINT ( 'NONE', #3675 ) ;
#13310 = DIRECTION ( 'NONE',  ( 0.000000000000000000, 0.000000000000000000, -1.000000000000000000 ) ) ;
#13311 = LINE ( 'NONE', #16818, #10185 ) ;
#13312 = CARTESIAN_POINT ( 'NONE',  ( -12.31900000000000084, -3661.486200000000281, 2249.723686796999573 ) ) ;
#13313 = AXIS2_PLACEMENT_3D ( 'NONE', #1724, #8872, #5828 ) ;
#13314 = B_SPLINE_CURVE_WITH_KNOTS ( 'NONE', 3,
 ( #3682, #12710, #14585, #11181, #2044, #16447, #9194, #21730, #515, #12821, #399, #19977, #21845, #7654, #5686, #5802, #14816, #16222, #12599, #5919, #16110, #14358 ),
 .UNSPECIFIED., .F., .F.,
 ( 4, 2, 2, 1, 2, 2, 2, 1, 2, 2, 2, 4 ),
 ( 0.000000000000000000, 0.1250000000017447987, 0.1875000000025351665, 0.2187500000028428926, 0.2343750000029967695, 0.2500000000031506464, 0.3750000000040985548, 0.4375000000042824078, 0.4687500000042232329, 0.5000000000041640025, 0.7500000000020820012, 1.000000000000000000 ),
 .UNSPECIFIED. ) ;
#13315 = ORIENTED_EDGE ( 'NONE', *, *, #6085, .F. ) ;
#13316 = VECTOR ( 'NONE', #13436, 1000.000000000000000 ) ;
#13317 = FACE_BOUND ( 'NONE', #3491, .T. ) ;
#13318 = AXIS2_PLACEMENT_3D ( 'NONE', #14125, #21034, #5102 ) ;
#13319 = CARTESIAN_POINT ( 'NONE',  ( 12.70000000028313281, -3656.372659094870869, 2239.009999999999764 ) ) ;
#13320 = CARTESIAN_POINT ( 'NONE',  ( 134.1946444147164925, -3577.961207644249043, 2244.692860678807392 ) ) ;
#13321 = ORIENTED_EDGE ( 'NONE', *, *, #1346, .T. ) ;
#13322 = CARTESIAN_POINT ( 'NONE',  ( -5.588000000000000078, -3694.938000000000102, 2229.612000000000080 ) ) ;
#13323 = EDGE_CURVE ( 'NONE', #7817, #15388, #14033, .T. ) ;
#13324 = CYLINDRICAL_SURFACE ( 'NONE', #19301, 0.7619999999999294005 ) ;
#13325 = CARTESIAN_POINT ( 'NONE',  ( 0.7620000000000000107, -3543.299999999999727, 2239.771999999999935 ) ) ;
#13326 = CIRCLE ( 'NONE', #4398, 2.844799999998842033 ) ;
#13327 = ORIENTED_EDGE ( 'NONE', *, *, #8095, .F. ) ;
#13328 = AXIS2_PLACEMENT_3D ( 'NONE', #6608, #11977, #22511 ) ;
#13329 = DIRECTION ( 'NONE',  ( 0.5000000000040877302, 0.8660254037820785955, 0.000000000000000000 ) ) ;
#13330 = DIRECTION ( 'NONE',  ( 0.000000000000000000, -1.000000000000000000, 0.000000000000000000 ) ) ;
#13331 = CARTESIAN_POINT ( 'NONE',  ( 38.10000000000000142, -3644.899999999999636, 2239.771999999999935 ) ) ;
#13332 = LINE ( 'NONE', #7948, #13935 ) ;
#13333 = ORIENTED_EDGE ( 'NONE', *, *, #13162, .F. ) ;
#13334 = AXIS2_PLACEMENT_3D ( 'NONE', #18116, #14500, #21641 ) ;
#13335 = ORIENTED_EDGE ( 'NONE', *, *, #21976, .F. ) ;
#13336 = PRODUCT_DEFINITION_SHAPE ( 'NONE', 'NONE',  #23166 ) ;
#13337 = CIRCLE ( 'NONE', #6614, 3.175000000000149925 ) ;
#13338 = CARTESIAN_POINT ( 'NONE',  ( 136.9873132030510305, -3657.938829547328169, 2239.009999999999764 ) ) ;
#13339 = ORIENTED_EDGE ( 'NONE', *, *, #13388, .T. ) ;
#13340 = CARTESIAN_POINT ( 'NONE',  ( 64.76999999999999602, -3695.699999999999818, 2289.213099999999940 ) ) ;
#13341 = APPLIED_PERSON_AND_ORGANIZATION_ASSIGNMENT ( #21308, #18241, ( #19492 ) ) ;
#13342 = CIRCLE ( 'NONE', #6246, 5.587999999999926359 ) ;
#13343 = CARTESIAN_POINT ( 'NONE',  ( 20.32000000000000028, -3670.300000000000182, 2289.213099999999940 ) ) ;
#13344 = CARTESIAN_POINT ( 'NONE',  ( 15.24000000000000021, -3694.430000000000291, 2255.774000000000342 ) ) ;
#13345 = CARTESIAN_POINT ( 'NONE',  ( 10.36831320283000046, -3640.848700000000008, 2292.781800000000203 ) ) ;
#13346 = LINE ( 'NONE', #1027, #11700 ) ;
#13347 = DIRECTION ( 'NONE',  ( 0.000000000000000000, 0.000000000000000000, -1.000000000000000000 ) ) ;
#13348 = VERTEX_POINT ( 'NONE', #12701 ) ;
#13349 = CARTESIAN_POINT ( 'NONE',  ( 12.70000000005999929, -3656.812599999999748, 2242.820000000000164 ) ) ;
#13350 = TOROIDAL_SURFACE ( 'NONE', #21228, 3.606799999999999784, 0.7620000000000000107 ) ;
#13351 = DIRECTION ( 'NONE',  ( 0.000000000000000000, 0.000000000000000000, -1.000000000000000000 ) ) ;
#13352 = VERTEX_POINT ( 'NONE', #10826 ) ;
#13353 = DIRECTION ( 'NONE',  ( 0.000000000000000000, -1.000000000000000000, 0.000000000000000000 ) ) ;
#13354 = CIRCLE ( 'NONE', #21952, 0.7619999999999294005 ) ;
#13355 = CARTESIAN_POINT ( 'NONE',  ( 139.8886820246942193, -3662.349796521664302, 2257.592643472502914 ) ) ;
#13356 = CIRCLE ( 'NONE', #14494, 3.175000000000149925 ) ;
#13357 = ORIENTED_EDGE ( 'NONE', *, *, #516, .F. ) ;
#13358 = ORIENTED_EDGE ( 'NONE', *, *, #6707, .T. ) ;
#13359 = AXIS2_PLACEMENT_3D ( 'NONE', #3235, #17523, #15779 ) ;
#13360 = EDGE_LOOP ( 'NONE', ( #9496, #7282, #19193, #5286, #2495, #4240, #11636, #8373 ) ) ;
#13361 = CYLINDRICAL_SURFACE ( 'NONE', #7194, 0.7619999999999996776 ) ;
#13362 = ORIENTED_EDGE ( 'NONE', *, *, #20578, .T. ) ;
#13363 = CARTESIAN_POINT ( 'NONE',  ( 6.222999999999998977, -3639.502500000000055, 2296.591799999999694 ) ) ;
#13364 = CARTESIAN_POINT ( 'NONE',  ( 11.80730815183341420, -3576.792673990085859, 2249.346535258006043 ) ) ;
#13365 = DIRECTION ( 'NONE',  ( 0.000000000000000000, 0.000000000000000000, 1.000000000000000000 ) ) ;
#13366 = CARTESIAN_POINT ( 'NONE',  ( 141.7296139770200512, -3581.488818245647053, 2248.480571682398477 ) ) ;
#13367 = ORIENTED_EDGE ( 'NONE', *, *, #20753, .F. ) ;
#13368 = CARTESIAN_POINT ( 'NONE',  ( 139.6999999999999886, -3656.329999999999472, 2270.760000000000218 ) ) ;
#13369 = COORDINATED_UNIVERSAL_TIME_OFFSET ( 0, 0, .AHEAD. ) ;
#13370 = APPLIED_PERSON_AND_ORGANIZATION_ASSIGNMENT ( #18236, #8562, ( #17087 ) ) ;
#13371 = AXIS2_PLACEMENT_3D ( 'NONE', #7411, #9169, #376 ) ;
#13372 = MANIFOLD_SOLID_BREP ( 'TORNILLO1[1]', #18098 ) ;
#13373 = DIRECTION ( 'NONE',  ( 0.000000000000000000, -1.000000000000000000, 0.000000000000000000 ) ) ;
#13374 = CARTESIAN_POINT ( 'NONE',  ( 131.5729205195000020, -3543.299999999999727, 2259.329999999999927 ) ) ;
#13375 = CARTESIAN_POINT ( 'NONE',  ( -12.54218463261975813, -3662.832400000410871, 2247.392000000001190 ) ) ;
#13376 = ADVANCED_FACE ( 'NONE', ( #395 ), #2039, .T. ) ;
#13377 = VECTOR ( 'NONE', #5172, 1000.000000000000000 ) ;
#13378 = EDGE_CURVE ( 'NONE', #11527, #12156, #18886, .T. ) ;
#13379 = ORIENTED_EDGE ( 'NONE', *, *, #4508, .F. ) ;
#13380 = CARTESIAN_POINT ( 'NONE',  ( 50.79999999999999716, -3670.300000000000182, 2239.771999999999935 ) ) ;
#13381 = EDGE_CURVE ( 'NONE', #16324, #7211, #5437, .T. ) ;
#13382 = ORIENTED_EDGE ( 'NONE', *, *, #14973, .F. ) ;
#13383 = ORIENTED_EDGE ( 'NONE', *, *, #18262, .F. ) ;
#13384 = ORIENTED_EDGE ( 'NONE', *, *, #4655, .T. ) ;
#13385 = CIRCLE ( 'NONE', #17889, 2.844799999998998796 ) ;
#13386 = DIRECTION ( 'NONE',  ( 0.000000000000000000, 0.000000000000000000, -1.000000000000000000 ) ) ;
#13387 = EDGE_LOOP ( 'NONE', ( #21507, #21892 ) ) ;
#13388 = EDGE_CURVE ( 'NONE', #19496, #16546, #21529, .T. ) ;
#13389 = DIRECTION ( 'NONE',  ( 0.000000000000000000, 0.000000000000000000, -1.000000000000000000 ) ) ;
#13390 = LINE ( 'NONE', #20419, #21513 ) ;
#13391 = ADVANCED_FACE ( 'NONE', ( #841 ), #11394, .T. ) ;
#13392 = ORIENTED_EDGE ( 'NONE', *, *, #22250, .F. ) ;
#13393 = CARTESIAN_POINT ( 'NONE',  ( 12.69999999999999929, -3599.497499999999945, 2263.571799999999712 ) ) ;
#13394 = DIRECTION ( 'NONE',  ( 0.5000000000005969669, -0.8660254037840939834, 0.000000000000000000 ) ) ;
#13395 = ADVANCED_FACE ( 'NONE', ( #9525 ), #18522, .T. ) ;
#13396 = FACE_OUTER_BOUND ( 'NONE', #22261, .T. ) ;
#13397 = DATE_AND_TIME ( #18663, #16497 ) ;
#13398 = CYLINDRICAL_SURFACE ( 'NONE', #12791, 2.844799999999999773 ) ;
#13399 = DIRECTION ( 'NONE',  ( -2.318894227180156550E-14, -1.000000000000000000, 0.000000000000000000 ) ) ;
#13400 = SHAPE_REPRESENTATION ( 'Roller 2', ( #5611 ), #11980 ) ;
#13401 = CARTESIAN_POINT ( 'NONE',  ( 133.9850000806000025, -3659.504501929000071, 2244.618659328000376 ) ) ;
#13402 = AXIS2_PLACEMENT_3D ( 'NONE', #14101, #20901, #13756 ) ;
#13403 = DIRECTION ( 'NONE',  ( 0.000000000000000000, 0.000000000000000000, -1.000000000000000000 ) ) ;
#13404 = ORIENTED_EDGE ( 'NONE', *, *, #20802, .F. ) ;
#13405 = CARTESIAN_POINT ( 'NONE',  ( 136.9962324742510305, -3543.632335308055644, 2255.363864800105603 ) ) ;
#13406 = EDGE_CURVE ( 'NONE', #10444, #4163, #6560, .T. ) ;
#13407 = EDGE_LOOP ( 'NONE', ( #7852, #16698, #10476, #8580 ) ) ;
#13408 = CARTESIAN_POINT ( 'NONE',  ( 139.6999999999999886, -3582.339799999999286, 2257.592639999999847 ) ) ;
#13409 = EDGE_CURVE ( 'NONE', #19558, #894, #13390, .T. ) ;
#13410 = EDGE_CURVE ( 'NONE', #15423, #1694, #6189, .T. ) ;
#13411 = CARTESIAN_POINT ( 'NONE',  ( 18.41519309055000164, -3659.504912144000173, 2244.618989493999834 ) ) ;
#13412 = VERTEX_POINT ( 'NONE', #510 ) ;
#13413 = ORIENTED_EDGE ( 'NONE', *, *, #9487, .T. ) ;
#13414 = DIRECTION ( 'NONE',  ( 1.000000000000000000, 0.000000000000000000, 0.000000000000000000 ) ) ;
#13415 = LINE ( 'NONE', #7803, #2422 ) ;
#13416 = CARTESIAN_POINT ( 'NONE',  ( 10.00591156675000093, -3600.429449278999982, 2279.486295382999742 ) ) ;
#13417 = CARTESIAN_POINT ( 'NONE',  ( 9.855200000000998273, -3579.494999999999891, 2256.063560000000052 ) ) ;
#13418 = DIRECTION ( 'NONE',  ( 0.000000000000000000, -2.336881798971000105E-14, 1.000000000000000000 ) ) ;
#13419 = AXIS2_PLACEMENT_3D ( 'NONE', #8636, #17410, #8530 ) ;
#13420 = CARTESIAN_POINT ( 'NONE',  ( 20.68889176940725605, -3695.652054061570652, 2259.675914647556056 ) ) ;
#13421 = ORIENTED_EDGE ( 'NONE', *, *, #9265, .T. ) ;
#13422 = COORDINATED_UNIVERSAL_TIME_OFFSET ( 0, 0, .AHEAD. ) ;
#13423 = CARTESIAN_POINT ( 'NONE',  ( 145.2144692705681450, -3658.007655502538455, 2245.504405415671954 ) ) ;
#13424 = ADVANCED_FACE ( 'NONE', ( #6256 ), #13155, .F. ) ;
#13425 = CARTESIAN_POINT ( 'NONE',  ( 9.908383082390907148, -3580.044228178761841, 2249.978629610284770 ) ) ;
#13426 = FACE_OUTER_BOUND ( 'NONE', #10861, .T. ) ;
#13427 = ORIENTED_EDGE ( 'NONE', *, *, #5806, .T. ) ;
#13428 = DIRECTION ( 'NONE',  ( 0.000000000000000000, 0.000000000000000000, -1.000000000000000000 ) ) ;
#13429 = PLANE ( 'NONE',  #3525 ) ;
#13430 = CARTESIAN_POINT ( 'NONE',  ( 145.1820664649105765, -3661.120306023109606, 2244.721041474187587 ) ) ;
#13431 = ORIENTED_EDGE ( 'NONE', *, *, #11024, .F. ) ;
#13432 = CIRCLE ( 'NONE', #5975, 5.714999999998998881 ) ;
#13433 = CARTESIAN_POINT ( 'NONE',  ( -8.890000000017000303, -3577.513800000000174, 2249.723686796999573 ) ) ;
#13434 = CARTESIAN_POINT ( 'NONE',  ( 15.39811514000335713, -3660.419159658365061, 2250.226394777855148 ) ) ;
#13435 = ADVANCED_FACE ( 'NONE', ( #4254 ), #16783, .F. ) ;
#13436 = DIRECTION ( 'NONE',  ( 0.000000000000000000, -1.000000000000000000, 0.000000000000000000 ) ) ;
#13437 = ORIENTED_EDGE ( 'NONE', *, *, #15232, .T. ) ;
#13438 = EDGE_CURVE ( 'NONE', #19601, #13554, #21163, .T. ) ;
#13439 = CARTESIAN_POINT ( 'NONE',  ( 22.00181536726000076, -3544.061999999999898, 2275.224984633000076 ) ) ;
#13440 = DIRECTION ( 'NONE',  ( 3.212101257670982882E-14, 0.5000000000050977000, 0.8660254037814953954 ) ) ;
#13441 = DIRECTION ( 'NONE',  ( 0.000000000000000000, 2.336881798971000105E-14, -1.000000000000000000 ) ) ;
#13442 = CARTESIAN_POINT ( 'NONE',  ( 15.46655083684568055, -3658.835041740453107, 2249.921457276668207 ) ) ;
#13443 = FACE_OUTER_BOUND ( 'NONE', #12063, .T. ) ;
#13444 = EDGE_CURVE ( 'NONE', #10237, #10059, #11049, .T. ) ;
#13445 = ORIENTED_EDGE ( 'NONE', *, *, #15739, .T. ) ;
#13446 = AXIS2_PLACEMENT_3D ( 'NONE', #17281, #10027, #8273 ) ;
#13447 = LINE ( 'NONE', #2557, #16907 ) ;
#13448 = ORIENTED_EDGE ( 'NONE', *, *, #8843, .T. ) ;
#13449 = VECTOR ( 'NONE', #22057, 1000.000000000000000 ) ;
#13450 = EDGE_CURVE ( 'NONE', #15441, #21028, #7685, .T. ) ;
#13451 = CARTESIAN_POINT ( 'NONE',  ( 145.1237722701461337, -3581.296112608482872, 2245.922901420255130 ) ) ;
#13452 = DATE_AND_TIME ( #8183, #15734 ) ;
#13453 = EDGE_CURVE ( 'NONE', #825, #11149, #1318, .T. ) ;
#13454 = EDGE_CURVE ( 'NONE', #6119, #20566, #2602, .T. ) ;
#13455 = DIRECTION ( 'NONE',  ( 0.000000000000000000, 0.000000000000000000, -1.000000000000000000 ) ) ;
#13456 = CARTESIAN_POINT ( 'NONE',  ( 18.13280299816700136, -3661.283447638940288, 2244.782395619060026 ) ) ;
#13457 = CARTESIAN_POINT ( 'NONE',  ( 14.50488223892000050, -3657.299998513999981, 2257.739442581999810 ) ) ;
#13458 = DIRECTION ( 'NONE',  ( -1.000000000000000000, 0.000000000000000000, 0.000000000000000000 ) ) ;
#13459 = DIRECTION ( 'NONE',  ( 1.000000000000000000, 0.000000000000000000, 0.000000000000000000 ) ) ;
#13460 = ORIENTED_EDGE ( 'NONE', *, *, #16700, .F. ) ;
#13461 = AXIS2_PLACEMENT_3D ( 'NONE', #8793, #23072, #1519 ) ;
#13462 = DIRECTION ( 'NONE',  ( 0.000000000000000000, 0.000000000000000000, -1.000000000000000000 ) ) ;
#13463 = CARTESIAN_POINT ( 'NONE',  ( 20.32000000000000028, -3578.860000000000127, 2247.392000000000280 ) ) ;
#13464 = ORIENTED_EDGE ( 'NONE', *, *, #526, .F. ) ;
#13465 = LOCAL_TIME ( 17, 37, 43.00000000000000000, #2142 ) ;
#13466 = CARTESIAN_POINT ( 'NONE',  ( 137.3683132029000262, -3578.148799999999937, 2242.820000000000164 ) ) ;
#13467 = CARTESIAN_POINT ( 'NONE',  ( 10.90866455802274082, -3657.294969492509153, 2247.463672662353474 ) ) ;
#13468 = ORIENTED_EDGE ( 'NONE', *, *, #3381, .T. ) ;
#13469 = ORIENTED_EDGE ( 'NONE', *, *, #19387, .T. ) ;
#13470 = VERTEX_POINT ( 'NONE', #18543 ) ;
#13471 = FACE_OUTER_BOUND ( 'NONE', #20420, .T. ) ;
#13472 = VERTEX_POINT ( 'NONE', #21946 ) ;
#13473 = LINE ( 'NONE', #9839, #2152 ) ;
#13474 = DIRECTION ( 'NONE',  ( 5.572969907074833723E-14, -1.000000000000000000, 0.000000000000000000 ) ) ;
#13475 = CARTESIAN_POINT ( 'NONE',  ( 141.5633583212279234, -3581.644791717248609, 2247.976212405268598 ) ) ;
#13476 = ORIENTED_EDGE ( 'NONE', *, *, #1779, .F. ) ;
#13477 = LINE ( 'NONE', #13246, #18602 ) ;
#13478 = APPROVAL_ROLE ( '' ) ;
#13479 = MANIFOLD_SOLID_BREP ( 'TORNILLO5[1]', #5003 ) ;
#13480 = DIRECTION ( 'NONE',  ( 0.000000000000000000, 0.000000000000000000, -1.000000000000000000 ) ) ;
#13481 = LOCAL_TIME ( 17, 37, 43.00000000000000000, #21333 ) ;
#13482 = DIRECTION ( 'NONE',  ( -1.000000000000000000, -1.202995631304000193E-14, 0.000000000000000000 ) ) ;
#13483 = APPLIED_APPROVAL_ASSIGNMENT ( #17514, ( #13121 ) ) ;
#13484 = DIRECTION ( 'NONE',  ( -1.000000000000000000, 0.000000000000000000, 0.000000000000000000 ) ) ;
#13485 = ORIENTED_EDGE ( 'NONE', *, *, #13936, .T. ) ;
#13486 = DIRECTION ( 'NONE',  ( 0.000000000000000000, 0.000000000000000000, 1.000000000000000000 ) ) ;
#13487 = ORIENTED_EDGE ( 'NONE', *, *, #5525, .T. ) ;
#13488 = ORIENTED_EDGE ( 'NONE', *, *, #20706, .T. ) ;
#13489 = APPROVAL ( #6144, 'UNSPECIFIED' ) ;
#13490 = DIRECTION ( 'NONE',  ( 0.000000000000000000, 0.000000000000000000, 1.000000000000000000 ) ) ;
#13491 = VERTEX_POINT ( 'NONE', #13050 ) ;
#13492 = APPLIED_APPROVAL_ASSIGNMENT ( #1885, ( #19492 ) ) ;
#13493 = FACE_OUTER_BOUND ( 'NONE', #5439, .T. ) ;
#13494 = DIRECTION ( 'NONE',  ( -0.7071067811865975328, 0.000000000000000000, -0.7071067811864976127 ) ) ;
#13495 = LOCAL_TIME ( 17, 37, 43.00000000000000000, #19627 ) ;
#13496 = VERTEX_POINT ( 'NONE', #20198 ) ;
#13497 = AXIS2_PLACEMENT_3D ( 'NONE', #5363, #5134, #1729 ) ;
#13498 = FACE_BOUND ( 'NONE', #17001, .T. ) ;
#13499 = EDGE_CURVE ( 'NONE', #16275, #21968, #22642, .T. ) ;
#13500 = CARTESIAN_POINT ( 'NONE',  ( -0.7620000000000000107, -3694.938000000000102, 2253.487999999999829 ) ) ;
#13501 = EDGE_CURVE ( 'NONE', #2000, #6875, #2076, .T. ) ;
#13502 = CARTESIAN_POINT ( 'NONE',  ( 11.34365660143000021, -3661.854255679000289, 2239.391000000000076 ) ) ;
#13503 = PERSON_AND_ORGANIZATION_ROLE ( 'creator' ) ;
#13504 = EDGE_CURVE ( 'NONE', #15888, #14896, #933, .T. ) ;
#13505 = AXIS2_PLACEMENT_3D ( 'NONE', #9551, #652, #7801 ) ;
#13506 = DIRECTION ( 'NONE',  ( 0.000000000000000000, 0.000000000000000000, 1.000000000000000000 ) ) ;
#13507 = DIRECTION ( 'NONE',  ( 0.000000000000000000, -1.000000000000000000, 0.000000000000000000 ) ) ;
#13508 = DIRECTION ( 'NONE',  ( 1.000000000000000000, 0.000000000000000000, 0.000000000000000000 ) ) ;
#13509 = CARTESIAN_POINT ( 'NONE',  ( 141.8306442670041179, -3657.619971841161714, 2248.712053168803322 ) ) ;
#13510 = DIRECTION ( 'NONE',  ( -1.000000000000000000, 0.000000000000000000, 2.324635735433000053E-14 ) ) ;
#13511 = EDGE_CURVE ( 'NONE', #1438, #17234, #15166, .T. ) ;
#13512 = LOCAL_TIME ( 17, 37, 43.00000000000000000, #5213 ) ;
#13513 = VERTEX_POINT ( 'NONE', #5065 ) ;
#13514 = CARTESIAN_POINT ( 'NONE',  ( 137.0287686657979407, -3543.717426572939530, 2255.445352725414068 ) ) ;
#13515 = MANIFOLD_SOLID_BREP ( 'SOLID2-13[1]', #11708 ) ;
#13516 = ORIENTED_EDGE ( 'NONE', *, *, #409, .F. ) ;
#13517 = EDGE_CURVE ( 'NONE', #3735, #17090, #21172, .T. ) ;
#13518 = ORIENTED_EDGE ( 'NONE', *, *, #6651, .F. ) ;
#13519 = FACE_OUTER_BOUND ( 'NONE', #16388, .T. ) ;
#13520 = PRODUCT_DEFINITION_SHAPE ( 'NONE', 'NONE',  #23177 ) ;
#13521 = CIRCLE ( 'NONE', #4915, 3.606799999998994366 ) ;
#13522 = LINE ( 'NONE', #20659, #12532 ) ;
#13523 = VERTEX_POINT ( 'NONE', #17240 ) ;
#13524 = ORIENTED_EDGE ( 'NONE', *, *, #7169, .F. ) ;
#13525 = FACE_OUTER_BOUND ( 'NONE', #14287, .T. ) ;
#13526 = CARTESIAN_POINT ( 'NONE',  ( 12.69999999999999929, -3599.497499999999945, 2263.571799999999712 ) ) ;
#13527 = CARTESIAN_POINT ( 'NONE',  ( 35.56000000000000227, -3568.700000000000273, 2244.547199999999975 ) ) ;
#13528 = ORIENTED_EDGE ( 'NONE', *, *, #13274, .T. ) ;
#13529 = CARTESIAN_POINT ( 'NONE',  ( 101.5999999999999943, -3670.300000000000182, 2239.771999999999935 ) ) ;
#13530 = CARTESIAN_POINT ( 'NONE',  ( 12.69999999999999929, -3570.287499999999909, 2257.592639999999847 ) ) ;
#13531 = CARTESIAN_POINT ( 'NONE',  ( 17.85473721720958551, -3577.030903703768217, 2245.207284487792549 ) ) ;
#13532 =( BOUNDED_CURVE ( )  B_SPLINE_CURVE ( 3, ( #16843, #20366, #7952, #13338 ),
 .UNSPECIFIED., .F., .T. ) 
 B_SPLINE_CURVE_WITH_KNOTS ( ( 4, 4 ),
 ( -2.664535259100375697E-14, 1.570796326393333997 ),
 .UNSPECIFIED. ) 
 CURVE ( )  GEOMETRIC_REPRESENTATION_ITEM ( )  RATIONAL_B_SPLINE_CURVE ( ( 1.000000000000000000, 0.8047378542190078976, 0.8047378542190078976, 1.000000000000000000 ) ) 
 REPRESENTATION_ITEM ( '' )  );
#13533 = CARTESIAN_POINT ( 'NONE',  ( 134.3871257470999865, -3581.600847139000052, 2246.630000000000109 ) ) ;
#13534 = EDGE_CURVE ( 'NONE', #7479, #13971, #6715, .T. ) ;
#13535 = ORIENTED_EDGE ( 'NONE', *, *, #20050, .F. ) ;
#13536 = PERSON_AND_ORGANIZATION_ROLE ( 'design_owner' ) ;
#13537 = ADVANCED_FACE ( 'NONE', ( #8229 ), #22627, .T. ) ;
#13538 = VERTEX_POINT ( 'NONE', #13973 ) ;
#13539 = CARTESIAN_POINT ( 'NONE',  ( 12.69999999999999929, -3602.672500000000127, 2264.841800000000148 ) ) ;
#13540 = CIRCLE ( 'NONE', #3436, 3.175000000000149925 ) ;
#13541 = TOROIDAL_SURFACE ( 'NONE', #14677, 3.606799999998999695, 0.7620000000000000107 ) ;
#13542 = CARTESIAN_POINT ( 'NONE',  ( 9.877889775156498686, -3579.858006066903272, 2250.056460527199306 ) ) ;
#13543 = CARTESIAN_POINT ( 'NONE',  ( 15.87499999973273823, -3543.615630734505885, 2281.351799999999912 ) ) ;
#13544 = EDGE_LOOP ( 'NONE', ( #16986, #9765 ) ) ;
#13545 = CYLINDRICAL_SURFACE ( 'NONE', #3218, 2.844799999998998796 ) ;
#13546 = ADVANCED_FACE ( 'NONE', ( #8470 ), #8812, .T. ) ;
#13547 = DIRECTION ( 'NONE',  ( 0.000000000000000000, -1.000000000000000000, 0.000000000000000000 ) ) ;
#13548 = FACE_BOUND ( 'NONE', #22873, .T. ) ;
#13549 = ORIENTED_EDGE ( 'NONE', *, *, #8556, .T. ) ;
#13550 = DIRECTION ( 'NONE',  ( 0.8928571428573600643, -0.4503400076038009403, 0.000000000000000000 ) ) ;
#13551 = AXIS2_PLACEMENT_3D ( 'NONE', #12511, #12632, #5496 ) ;
#13552 = FACE_OUTER_BOUND ( 'NONE', #3755, .T. ) ;
#13553 = CARTESIAN_POINT ( 'NONE',  ( 12.69999999999999929, -3664.965999999999894, 2245.359999999999673 ) ) ;
#13554 = VERTEX_POINT ( 'NONE', #19125 ) ;
#13555 = AXIS2_PLACEMENT_3D ( 'NONE', #23068, #4921, #17331 ) ;
#13556 = B_SPLINE_CURVE_WITH_KNOTS ( 'NONE', 3,
 ( #18838, #15795, #13921, #8299, #4657, #14039, #17541, #21070, #1486, #22921, #18962, #2906, #15444, #10164, #17304, #8414, #5606, #12630, #7241, #16028, #3596, #21538, #23044, #10754 ),
 .UNSPECIFIED., .F., .F.,
 ( 4, 2, 2, 1, 1, 1, 2, 2, 2, 2, 1, 2, 2, 4 ),
 ( 0.000000000000000000, 0.1249999999954432839, 0.1874999999933733841, 0.2187499999923384342, 0.2343749999923080418, 0.2421874999926629524, 0.2460937499926816874, 0.2499999999927004501, 0.3749999999974015785, 0.4374999999999966138, 0.4687500000008462120, 0.4843750000012573276, 0.5000000000016684432, 1.000000000000000000 ),
 .UNSPECIFIED. ) ;
#13557 = DIRECTION ( 'NONE',  ( -0.7071067811865975328, 0.000000000000000000, 0.7071067811864976127 ) ) ;
#13558 = CARTESIAN_POINT ( 'NONE',  ( 12.80540911176311170, -3636.657697124182050, 2279.817639555324149 ) ) ;
#13559 = VECTOR ( 'NONE', #21531, 1000.000000000000000 ) ;
#13560 = MANIFOLD_SOLID_BREP ( 'TORNILLO4[1]', #3489 ) ;
#13561 = LINE ( 'NONE', #22690, #6710 ) ;
#13562 = CARTESIAN_POINT ( 'NONE',  ( 15.52417949512691386, -3659.157734418582550, 2250.062346885889838 ) ) ;
#13563 = CARTESIAN_POINT ( 'NONE',  ( 15.03168679717000167, -3580.841199999999844, 2242.820000000000164 ) ) ;
#13564 = ORIENTED_EDGE ( 'NONE', *, *, #14409, .F. ) ;
#13565 = VERTEX_POINT ( 'NONE', #6947 ) ;
#13566 = ORIENTED_EDGE ( 'NONE', *, *, #7701, .T. ) ;
#13567 = CARTESIAN_POINT ( 'NONE',  ( 142.0316867971999955, -3578.148799999999937, 2242.820000000000164 ) ) ;
#13568 = ORIENTED_EDGE ( 'NONE', *, *, #2158, .F. ) ;
#13569 = CARTESIAN_POINT ( 'NONE',  ( 15.54479926893309027, -3579.587001414151928, 2257.962943127797644 ) ) ;
#13571 = CIRCLE ( 'NONE', #15814, 5.460999999999938126 ) ;
#13570 = APPROVAL_ROLE ( '' ) ;
#13572 = EDGE_CURVE ( 'NONE', #10769, #20632, #5061, .T. ) ;
#13573 = DIRECTION ( 'NONE',  ( 1.000000000000000000, 0.000000000000000000, 0.000000000000000000 ) ) ;
#13574 = ADVANCED_FACE ( 'NONE', ( #8696, #15617 ), #11972, .F. ) ;
#13575 = CARTESIAN_POINT ( 'NONE',  ( 105.2067999999999870, -3619.500000000000000, 2260.600000000000364 ) ) ;
#13576 = ADVANCED_FACE ( 'NONE', ( #1071 ), #13853, .F. ) ;
#13577 = CARTESIAN_POINT ( 'NONE',  ( 11.36465921565999970, -3662.022152739999456, 2257.672217410000030 ) ) ;
#13578 = AXIS2_PLACEMENT_3D ( 'NONE', #6773, #13913, #21065 ) ;
#13579 = CARTESIAN_POINT ( 'NONE',  ( 139.7000000001000046, -3576.802599999999984, 2242.820000000000164 ) ) ;
#13580 = CARTESIAN_POINT ( 'NONE',  ( 10.36831320284000135, -3638.156300000000101, 2292.781800000000203 ) ) ;
#13581 = VECTOR ( 'NONE', #4002, 999.9999999999998863 ) ;
#13582 = DIRECTION ( 'NONE',  ( 0.000000000000000000, 0.000000000000000000, -1.000000000000000000 ) ) ;
#13583 = EDGE_CURVE ( 'NONE', #4126, #5555, #19284, .T. ) ;
#13584 = ORIENTED_EDGE ( 'NONE', *, *, #11432, .T. ) ;
#13585 = CARTESIAN_POINT ( 'NONE',  ( 7.387125747152000876, -3657.399152860999493, 2246.630000000000109 ) ) ;
#13586 = CYLINDRICAL_SURFACE ( 'NONE', #14436, 2.844799999998995244 ) ;
#13587 = ORIENTED_EDGE ( 'NONE', *, *, #19543, .F. ) ;
#13588 = LINE ( 'NONE', #20853, #8809 ) ;
#13589 = CARTESIAN_POINT ( 'NONE',  ( 10.23711275231256579, -3658.078120033774667, 2249.355894016820912 ) ) ;
#13590 = EDGE_CURVE ( 'NONE', #17865, #553, #10679, .T. ) ;
#13591 = ORIENTED_EDGE ( 'NONE', *, *, #16111, .F. ) ;
#13592 = ADVANCED_FACE ( 'NONE', ( #14090 ), #5189, .F. ) ;
#13593 = ORIENTED_EDGE ( 'NONE', *, *, #13869, .T. ) ;
#13594 = CARTESIAN_POINT ( 'NONE',  ( 134.2318573182560897, -3581.156156794382241, 2245.707491121732346 ) ) ;
#13595 = EDGE_LOOP ( 'NONE', ( #21491, #14220, #18954, #12328 ) ) ;
#13596 = CLOSED_SHELL ( 'NONE', ( #5156, #22047, #8676, #4480, #2355, #21118, #13664, #6931, #7281, #976, #12795, #12286, #7585, #18965, #10089, #20536, #8416, #19291, #21827, #14620, #21461, #19087, #13574, #4973, #297, #21566 ) ) ;
#13597 = CARTESIAN_POINT ( 'NONE',  ( -8.890000000022000748, -3661.486200000000281, 2245.060313203000078 ) ) ;
#13598 = DIRECTION ( 'NONE',  ( -0.000000000000000000, -1.000000000000000000, -0.000000000000000000 ) ) ;
#13599 = DIRECTION ( 'NONE',  ( 0.000000000000000000, 0.000000000000000000, 1.000000000000000000 ) ) ;
#13600 = CARTESIAN_POINT ( 'NONE',  ( 142.0697870230637818, -3581.068730170725303, 2249.184906718528509 ) ) ;
#13601 = ORIENTED_EDGE ( 'NONE', *, *, #5241, .F. ) ;
#13602 = CARTESIAN_POINT ( 'NONE',  ( 138.2712681479159471, -3581.962087688927568, 2257.683753140937824 ) ) ;
#13603 = DATE_AND_TIME ( #1164, #13842 ) ;
#13604 = ADVANCED_FACE ( 'NONE', ( #9979 ), #22256, .T. ) ;
#13605 = FACE_OUTER_BOUND ( 'NONE', #10120, .T. ) ;
#13606 = CARTESIAN_POINT ( 'NONE',  ( 20.82707948048999924, -3543.299999999999727, 2259.329999999999927 ) ) ;
#13607 = CIRCLE ( 'NONE', #13228, 2.844799999999999773 ) ;
#13608 = CARTESIAN_POINT ( 'NONE',  ( 134.1359104811938892, -3658.200395526626835, 2245.310932276000585 ) ) ;
#13609 = EDGE_LOOP ( 'NONE', ( #15474, #5382, #19771, #9799 ) ) ;
#13610 = CARTESIAN_POINT ( 'NONE',  ( -12.69999999999999929, -3580.426170453010855, 2250.104686796980332 ) ) ;
#13611 = AXIS2_PLACEMENT_3D ( 'NONE', #7746, #14898, #22025 ) ;
#13612 = ORIENTED_EDGE ( 'NONE', *, *, #22679, .F. ) ;
#13613 = CARTESIAN_POINT ( 'NONE',  ( 15.03168679717000167, -3580.841199999999844, 2239.391000000000076 ) ) ;
#13614 = CARTESIAN_POINT ( 'NONE',  ( 12.69999999976724148, -3662.637340905157544, 2239.009999999999764 ) ) ;
#13615 = EDGE_LOOP ( 'NONE', ( #23098, #21181, #5297, #20263, #12803, #499 ) ) ;
#13616 = CARTESIAN_POINT ( 'NONE',  ( 0.7620000000000000107, -3694.938000000000102, 2239.771999999999935 ) ) ;
#13617 = DIRECTION ( 'NONE',  ( 0.000000000000000000, 0.000000000000000000, -1.000000000000000000 ) ) ;
#13618 = TOROIDAL_SURFACE ( 'NONE', #2752, 3.606799999998999695, 0.7620000000000000107 ) ;
#13619 = ORIENTED_EDGE ( 'NONE', *, *, #9245, .T. ) ;
#13620 = DIRECTION ( 'NONE',  ( 0.5000000000031962211, 0.8660254037825932949, 0.000000000000000000 ) ) ;
#13621 =( LENGTH_UNIT ( ) NAMED_UNIT ( * ) SI_UNIT ( .MILLI., .METRE. ) );
#13622 = CARTESIAN_POINT ( 'NONE',  ( 13.32717070831999884, -3602.278331858999991, 2279.801370659999975 ) ) ;
#13623 = CARTESIAN_POINT ( 'NONE',  ( 63.50000000000000000, -3594.099999999999909, 2239.771999999999935 ) ) ;
#13624 = APPROVAL_STATUS ( 'not_yet_approved' ) ;
#13625 = LINE ( 'NONE', #19254, #8076 ) ;
#13626 = DIRECTION ( 'NONE',  ( 0.000000000000000000, 0.000000000000000000, -1.000000000000000000 ) ) ;
#13627 = DIRECTION ( 'NONE',  ( 1.000000000000000000, 0.000000000000000000, 0.000000000000000000 ) ) ;
#13628 = APPLIED_DATE_AND_TIME_ASSIGNMENT ( #15938, #17569, ( #22639 ) ) ;
#13629 = CARTESIAN_POINT ( 'NONE',  ( 141.4907929136770690, -3657.294513356050174, 2247.445207560118433 ) ) ;
#13630 = DIRECTION ( 'NONE',  ( 0.000000000000000000, 1.000000000000000000, 0.000000000000000000 ) ) ;
#13631 = EDGE_LOOP ( 'NONE', ( #19444, #9325, #13915, #19385, #3131 ) ) ;
#13632 = TOROIDAL_SURFACE ( 'NONE', #6538, 3.606799999999999784, 0.7620000000000000107 ) ;
#13633 = CARTESIAN_POINT ( 'NONE',  ( 137.1599999998475425, -3544.490134410746577, 2255.773999999840271 ) ) ;
#13634 = AXIS2_PLACEMENT_3D ( 'NONE', #10738, #17883, #1828 ) ;
#13635 = ADVANCED_FACE ( 'NONE', ( #10094 ), #3647, .F. ) ;
#13636 = AXIS2_PLACEMENT_3D ( 'NONE', #10854, #3815, #2865 ) ;
#13637 = ORIENTED_EDGE ( 'NONE', *, *, #21485, .F. ) ;
#13638 = DIRECTION ( 'NONE',  ( -1.000000000000000000, 0.000000000000000000, 0.000000000000000000 ) ) ;
#13639 = EDGE_CURVE ( 'NONE', #2680, #2712, #3940, .T. ) ;
#13640 = CARTESIAN_POINT ( 'NONE',  ( 12.70000000000017693, -3662.679999999999836, 2245.359999999999673 ) ) ;
#13641 = ORIENTED_EDGE ( 'NONE', *, *, #14366, .T. ) ;
#13642 = EDGE_LOOP ( 'NONE', ( #5953, #12994, #6589, #3339 ) ) ;
#13643 = CARTESIAN_POINT ( 'NONE',  ( 12.69999999999999929, -3579.494999999999891, 2272.030000000000200 ) ) ;
#13644 = DIRECTION ( 'NONE',  ( 0.000000000000000000, 0.000000000000000000, -1.000000000000000000 ) ) ;
#13645 = CYLINDRICAL_SURFACE ( 'NONE', #21190, 0.7619999999999241824 ) ;
#13646 = VERTEX_POINT ( 'NONE', #7404 ) ;
#13647 = CARTESIAN_POINT ( 'NONE',  ( 25.39999999999999858, -3660.140000000000327, 2247.392000000000280 ) ) ;
#13648 = CARTESIAN_POINT ( 'NONE',  ( 139.6999999999999886, -3579.494999999999891, 2239.009999999999764 ) ) ;
#13649 = CARTESIAN_POINT ( 'NONE',  ( 12.69999999999999929, -3579.494999999999891, 2245.359999999999673 ) ) ;
#13650 = AXIS2_PLACEMENT_3D ( 'NONE', #5937, #17149, #4279 ) ;
#13651 = CARTESIAN_POINT ( 'NONE',  ( 35.56000000000000227, -3670.300000000000182, 2247.392000000000280 ) ) ;
#13652 = CIRCLE ( 'NONE', #3544, 2.844800000000091700 ) ;
#13653 = CARTESIAN_POINT ( 'NONE',  ( 15.41268679701173738, -3597.931329547518999, 2296.591799999999694 ) ) ;
#13654 = EDGE_LOOP ( 'NONE', ( #20546, #13059, #17269, #9200, #8785, #10805 ) ) ;
#13655 = DATE_AND_TIME ( #12252, #20603 ) ;
#13656 = AXIS2_PLACEMENT_3D ( 'NONE', #9470, #563, #9246 ) ;
#13657 = ORIENTED_EDGE ( 'NONE', *, *, #11776, .F. ) ;
#13658 = CARTESIAN_POINT ( 'NONE',  ( 10.36831320290272984, -3638.156299999887324, 2296.210799999999836 ) ) ;
#13659 = APPLIED_PERSON_AND_ORGANIZATION_ASSIGNMENT ( #6398, #15651, ( #5365 ) ) ;
#13660 = CARTESIAN_POINT ( 'NONE',  ( 10.79725788089033855, -3581.609851679345411, 2248.121171040608260 ) ) ;
#13661 = FACE_OUTER_BOUND ( 'NONE', #3777, .T. ) ;
#13662 = VERTEX_POINT ( 'NONE', #14555 ) ;
#13663 = CARTESIAN_POINT ( 'NONE',  ( 12.69999999999999929, -3639.502500000000055, 2290.241799999999785 ) ) ;
#13664 = ADVANCED_FACE ( 'NONE', ( #17831 ), #2013, .F. ) ;
#13665 = B_SPLINE_CURVE_WITH_KNOTS ( 'NONE', 3,
 ( #10966, #14496, #16357, #3929, #19879, #2185, #11195, #310, #16241, #19770, #7342, #9331, #20115, #3811, #16466, #14724, #4049, #19640, #17885, #8979, #16127, #75, #2405, #16696, #13291, #18909, #11304, #17030, #747, #4162, #648, #15060, #18455, #11633, #2861, #4498, #15287, #18791, #13411 ),
 .UNSPECIFIED., .F., .F.,
 ( 4, 2, 2, 1, 1, 1, 2, 2, 2, 2, 2, 2, 1, 1, 2, 2, 2, 2, 1, 1, 2, 2, 4 ),
 ( 0.000000000000000000, 0.1250000000158134339, 0.1875000000236058673, 0.2187500000277668721, 0.2343750000298476244, 0.2421875000311433102, 0.2460937500318851334, 0.2500000000326269567, 0.3125000000339349104, 0.3750000000352428087, 0.4375000000365507624, 0.4687500000372124553, 0.4843750000373662767, 0.4921875000372503139, 0.4960937500371923048, 0.5000000000371342956, 0.6250000000314543946, 0.6875000000287884161, 0.7187500000274557044, 0.7343750000266703326, 0.7421875000260601540, 0.7500000000254499755, 1.000000000000000000 ),
 .UNSPECIFIED. ) ;
#13666 = CARTESIAN_POINT ( 'NONE',  ( 139.6999999999999886, -3668.712499999999636, 2268.705139999999574 ) ) ;
#13667 = CARTESIAN_POINT ( 'NONE',  ( 145.1350961731654365, -3661.271952279658763, 2244.781081194931630 ) ) ;
#13668 = CARTESIAN_POINT ( 'NONE',  ( 12.69999999999999929, -3659.504999999999654, 2244.978999999999814 ) ) ;
#13669 = TOROIDAL_SURFACE ( 'NONE', #17401, 5.080000000000000071, 0.3810000000000000053 ) ;
#13670 = FACE_OUTER_BOUND ( 'NONE', #8377, .T. ) ;
#13672 = ADVANCED_FACE ( 'NONE', ( #1888 ), #19940, .T. ) ;
#13671 = VECTOR ( 'NONE', #4424, 1000.000000000000000 ) ;
#13673 = DIRECTION ( 'NONE',  ( 0.000000000000000000, 0.000000000000000000, 1.000000000000000000 ) ) ;
#13674 = AXIS2_PLACEMENT_3D ( 'NONE', #21241, #15376, #21001 ) ;
#13675 = ORIENTED_EDGE ( 'NONE', *, *, #6301, .T. ) ;
#13676 = FACE_OUTER_BOUND ( 'NONE', #23114, .T. ) ;
#13677 = CARTESIAN_POINT ( 'NONE',  ( 139.6999999999999886, -3570.287499999999909, 2279.817639999999756 ) ) ;
#13678 = CARTESIAN_POINT ( 'NONE',  ( 104.4447999999999865, -3670.300000000000182, 2259.837999999999738 ) ) ;
#13679 = CARTESIAN_POINT ( 'NONE',  ( 15.54478936534684941, -3659.505023738319323, 2250.165136749944850 ) ) ;
#13680 = CARTESIAN_POINT ( 'NONE',  ( 12.69999999999999929, -3649.471999999999753, 2275.055139999999483 ) ) ;
#13681 = VERTEX_POINT ( 'NONE', #9280 ) ;
#13682 = EDGE_CURVE ( 'NONE', #10278, #13993, #1652, .T. ) ;
#13683 = EDGE_LOOP ( 'NONE', ( #17707, #12301, #1670, #8351 ) ) ;
#13684 = CARTESIAN_POINT ( 'NONE',  ( 116.8400000000000034, -3695.699999999999818, 2243.277199999999993 ) ) ;
#13685 = EDGE_CURVE ( 'NONE', #12882, #20359, #12442, .T. ) ;
#13686 = VECTOR ( 'NONE', #1595, 1000.000000000000000 ) ;
#13687 = EDGE_LOOP ( 'NONE', ( #1698, #19447, #17211, #20284, #17726, #4812 ) ) ;
#13688 = CARTESIAN_POINT ( 'NONE',  ( 15.49598722424000030, -3580.043501552999714, 2257.950090894999903 ) ) ;
#13689 = SECURITY_CLASSIFICATION_LEVEL ( 'unclassified' ) ;
#13690 = DIRECTION ( 'NONE',  ( 0.000000000000000000, 1.000000000000000000, 0.000000000000000000 ) ) ;
#13691 = AXIS2_PLACEMENT_3D ( 'NONE', #5254, #19545, #8888 ) ;
#13692 = ORIENTED_EDGE ( 'NONE', *, *, #19599, .T. ) ;
#13693 = AXIS2_PLACEMENT_3D ( 'NONE', #10878, #15316, #22213 ) ;
#13694 = DIRECTION ( 'NONE',  ( -0.000000000000000000, -1.000000000000000000, -0.000000000000000000 ) ) ;
#13695 = DIRECTION ( 'NONE',  ( 1.000000000000000000, 0.000000000000000000, -2.336881798971000105E-14 ) ) ;
#13696 = CYLINDRICAL_SURFACE ( 'NONE', #1375, 6.349999999999855760 ) ;
#13697 = DIRECTION ( 'NONE',  ( 0.000000000000000000, 0.000000000000000000, -1.000000000000000000 ) ) ;
#13698 = VECTOR ( 'NONE', #11709, 1000.000000000000000 ) ;
#13699 = CARTESIAN_POINT ( 'NONE',  ( 137.5031457249828577, -3577.685606708022533, 2249.984038353326014 ) ) ;
#13700 = ORIENTED_EDGE ( 'NONE', *, *, #15602, .F. ) ;
#13701 = DIRECTION ( 'NONE',  ( 0.000000000000000000, 0.000000000000000000, -1.000000000000000000 ) ) ;
#13702 = ADVANCED_FACE ( 'NONE', ( #16414 ), #16071, .T. ) ;
#13703 = DIRECTION ( 'NONE',  ( -1.000000000000000000, -1.165588477296754225E-12, 0.000000000000000000 ) ) ;
#13704 = ORIENTED_EDGE ( 'NONE', *, *, #2643, .T. ) ;
#13705 = VECTOR ( 'NONE', #5333, 1000.000000000000000 ) ;
#13706 = CIRCLE ( 'NONE', #11455, 5.080000000000000959 ) ;
#13707 = DIRECTION ( 'NONE',  ( 0.000000000000000000, 0.000000000000000000, -1.000000000000000000 ) ) ;
#13708 = AXIS2_PLACEMENT_3D ( 'NONE', #8254, #9665, #15403 ) ;
#13709 = ADVANCED_FACE ( 'NONE', ( #19472, #14324 ), #14441, .T. ) ;
#13710 = ORIENTED_EDGE ( 'NONE', *, *, #19872, .T. ) ;
#13711 = AXIS2_PLACEMENT_3D ( 'NONE', #58, #12708, #9077 ) ;
#13712 = EDGE_CURVE ( 'NONE', #8893, #2492, #15549, .T. ) ;
#13713 = ORIENTED_EDGE ( 'NONE', *, *, #13208, .F. ) ;
#13714 = CARTESIAN_POINT ( 'NONE',  ( 123.3932000000010021, -3670.300000000000182, 2259.837999999999738 ) ) ;
#13715 = CIRCLE ( 'NONE', #15955, 3.175000000000149925 ) ;
#13716 = VERTEX_POINT ( 'NONE', #12673 ) ;
#13717 = DIRECTION ( 'NONE',  ( 9.713237310828999775E-14, 5.180393232441999927E-13, 1.000000000000000000 ) ) ;
#13718 = DIRECTION ( 'NONE',  ( 0.000000000000000000, 1.000000000000000000, 0.000000000000000000 ) ) ;
#13719 = DIRECTION ( 'NONE',  ( 1.000000000000000000, 0.000000000000000000, 0.000000000000000000 ) ) ;
#13720 = CIRCLE ( 'NONE', #12227, 5.460999999999938126 ) ;
#13721 = CARTESIAN_POINT ( 'NONE',  ( 15.74707948048999917, -3543.299999999999727, 2254.503999999999905 ) ) ;
#13722 = ORIENTED_EDGE ( 'NONE', *, *, #1557, .F. ) ;
#13723 = CARTESIAN_POINT ( 'NONE',  ( 131.7496328904776988, -3695.620464488476500, 2259.772527316505148 ) ) ;
#13724 = DATE_AND_TIME ( #8211, #11582 ) ;
#13725 = CARTESIAN_POINT ( 'NONE',  ( 142.0316867971999955, -3658.158799999999701, 2239.391000000000076 ) ) ;
#13726 = CARTESIAN_POINT ( 'NONE',  ( 14.61268103042000099, -3581.600842893000390, 2246.630000000000109 ) ) ;
#13727 = EDGE_CURVE ( 'NONE', #2186, #19565, #200, .T. ) ;
#13728 = CARTESIAN_POINT ( 'NONE',  ( 134.2666750161357072, -3657.732842303892539, 2245.875864816541252 ) ) ;
#13729 = CIRCLE ( 'NONE', #4011, 0.7619999999999294005 ) ;
#13730 = ORIENTED_EDGE ( 'NONE', *, *, #1463, .F. ) ;
#13731 = CIRCLE ( 'NONE', #12981, 2.844799999998998796 ) ;
#13732 = CARTESIAN_POINT ( 'NONE',  ( 15.51380746874810335, -3695.561367820956548, 2255.088321283119967 ) ) ;
#13733 = AXIS2_PLACEMENT_3D ( 'NONE', #7338, #21635, #16575 ) ;
#13734 = ORIENTED_EDGE ( 'NONE', *, *, #21910, .F. ) ;
#13735 = LINE ( 'NONE', #19116, #14782 ) ;
#13736 = ORIENTED_EDGE ( 'NONE', *, *, #5992, .T. ) ;
#13737 = CARTESIAN_POINT ( 'NONE',  ( -0.7620000000000000107, -3543.299999999999727, 2239.771999999999935 ) ) ;
#13738 = EDGE_CURVE ( 'NONE', #7229, #12882, #19665, .T. ) ;
#13739 = DIRECTION ( 'NONE',  ( 0.000000000000000000, 0.000000000000000000, -1.000000000000000000 ) ) ;
#13740 = EDGE_LOOP ( 'NONE', ( #1006, #9727 ) ) ;
#13741 = ORIENTED_EDGE ( 'NONE', *, *, #22969, .T. ) ;
#13742 = FACE_OUTER_BOUND ( 'NONE', #23122, .T. ) ;
#13743 = DIRECTION ( 'NONE',  ( 0.000000000000000000, -1.000000000000000000, 0.000000000000000000 ) ) ;
#13744 = AXIS2_PLACEMENT_3D ( 'NONE', #3511, #123, #3980 ) ;
#13745 = ORIENTED_EDGE ( 'NONE', *, *, #17387, .T. ) ;
#13746 = AXIS2_PLACEMENT_3D ( 'NONE', #9047, #9288, #4009 ) ;
#13747 = PLANE ( 'NONE',  #3102 ) ;
#13748 = CARTESIAN_POINT ( 'NONE',  ( -12.69999999999999929, -3657.007659095000236, 2247.392000000000280 ) ) ;
#13749 =( NAMED_UNIT ( * ) SI_UNIT ( $, .STERADIAN. ) SOLID_ANGLE_UNIT ( ) );
#13750 = FACE_OUTER_BOUND ( 'NONE', #7378, .T. ) ;
#13751 = CARTESIAN_POINT ( 'NONE',  ( 136.9269754645999910, -3578.860002036999958, 2250.236803302000226 ) ) ;
#13752 = PERSON_AND_ORGANIZATION ( #5446, #1895 ) ;
#13753 = AXIS2_PLACEMENT_3D ( 'NONE', #16463, #417, #21966 ) ;
#13754 = CARTESIAN_POINT ( 'NONE',  ( 20.32000000000000028, -3576.955000000000382, 2247.392000000000280 ) ) ;
#13755 = CARTESIAN_POINT ( 'NONE',  ( 14.61268103042000099, -3581.600842893000390, 2246.630000000000109 ) ) ;
#13756 = DIRECTION ( 'NONE',  ( -1.000000000000000000, 0.000000000000000000, 0.000000000000000000 ) ) ;
#13757 = ADVANCED_FACE ( 'NONE', ( #21468 ), #4687, .T. ) ;
#13758 = CARTESIAN_POINT ( 'NONE',  ( 142.1353304486877391, -3658.034425628051395, 2249.305387334696661 ) ) ;
#13759 = VERTEX_POINT ( 'NONE', #17706 ) ;
#13760 = CARTESIAN_POINT ( 'NONE',  ( 136.8684679650089038, -3543.420329759140259, 2255.043779574668406 ) ) ;
#13761 = VECTOR ( 'NONE', #3829, 1000.000000000000000 ) ;
#13762 = ORIENTED_EDGE ( 'NONE', *, *, #12927, .F. ) ;
#13763 = ORIENTED_EDGE ( 'NONE', *, *, #6579, .F. ) ;
#13764 = CARTESIAN_POINT ( 'NONE',  ( -5.588000000000000078, -3660.140000000000327, 2250.236800000000130 ) ) ;
#13765 = VECTOR ( 'NONE', #19759, 1000.000000000000000 ) ;
#13766 = DIRECTION ( 'NONE',  ( 0.000000000000000000, 0.000000000000000000, 1.000000000000000000 ) ) ;
#13767 = VERTEX_POINT ( 'NONE', #14207 ) ;
#13768 = ORIENTED_EDGE ( 'NONE', *, *, #16938, .F. ) ;
#13769 = CARTESIAN_POINT ( 'NONE',  ( 4.743095773629126377, -3543.373434456934774, 2259.755879528988771 ) ) ;
#13770 = CARTESIAN_POINT ( 'NONE',  ( 76.20000000000000284, -3670.300000000000182, 2260.600000000000364 ) ) ;
#13771 = LINE ( 'NONE', #23002, #14832 ) ;
#13772 = APPLIED_DATE_AND_TIME_ASSIGNMENT ( #8726, #17618, ( #9398 ) ) ;
#13773 = EDGE_LOOP ( 'NONE', ( #16350, #3290, #1980, #12556, #7448 ) ) ;
#13774 = DIRECTION ( 'NONE',  ( 0.000000000000000000, -1.000000000000000000, 0.000000000000000000 ) ) ;
#13775 = DIRECTION ( 'NONE',  ( -0.8928571428563427670, 0.4503400076058181045, 0.000000000000000000 ) ) ;
#13776 = CARTESIAN_POINT ( 'NONE',  ( 10.36831320285999958, -3578.148799999999937, 2242.820000000000164 ) ) ;
#13777 = CARTESIAN_POINT ( 'NONE',  ( 138.4364504584586655, -3656.949413510948489, 2257.663356986367944 ) ) ;
#13778 = CARTESIAN_POINT ( 'NONE',  ( 9.525000000091798924, -3694.938000000000102, 2281.351800000090861 ) ) ;
#13779 = ORIENTED_EDGE ( 'NONE', *, *, #18021, .F. ) ;
#13780 = COORDINATED_UNIVERSAL_TIME_OFFSET ( 0, 0, .AHEAD. ) ;
#13781 = AXIS2_PLACEMENT_3D ( 'NONE', #1667, #15856, #10581 ) ;
#13782 = VERTEX_POINT ( 'NONE', #21353 ) ;
#13783 = CARTESIAN_POINT ( 'NONE',  ( 12.69999999999999929, -3599.497499999999945, 2296.591799999999694 ) ) ;
#13784 = CARTESIAN_POINT ( 'NONE',  ( 10.79145926739417760, -3581.604639450296872, 2248.140541687839232 ) ) ;
#13785 = ORIENTED_EDGE ( 'NONE', *, *, #20587, .T. ) ;
#13786 = DIRECTION ( 'NONE',  ( 0.000000000000000000, 0.000000000000000000, 1.000000000000000000 ) ) ;
#13787 = VERTEX_POINT ( 'NONE', #19592 ) ;
#13788 = DIRECTION ( 'NONE',  ( -1.000000000000000000, 0.000000000000000000, 0.000000000000000000 ) ) ;
#13789 = EDGE_LOOP ( 'NONE', ( #21552, #11563, #2517, #4135 ) ) ;
#13790 = CARTESIAN_POINT ( 'NONE',  ( 64.76999999999999602, -3694.938000000000102, 2285.606299999999919 ) ) ;
#13791 = CARTESIAN_POINT ( 'NONE',  ( 15.03168679714000078, -3638.156300000000101, 2292.781800000000203 ) ) ;
#13792 = CARTESIAN_POINT ( 'NONE',  ( 11.20651475058533464, -3661.926271786974212, 2249.606089457644430 ) ) ;
#13793 = CARTESIAN_POINT ( 'NONE',  ( 147.4346858863133320, -3543.765301129279123, 2260.312744311644565 ) ) ;
#13794 = ORIENTED_EDGE ( 'NONE', *, *, #23162, .F. ) ;
#13795 = DIRECTION ( 'NONE',  ( -1.000000000000000000, 0.000000000000000000, 0.000000000000000000 ) ) ;
#13796 = CARTESIAN_POINT ( 'NONE',  ( 12.69999999999999929, -3659.504999999999654, 2272.030000000000200 ) ) ;
#13797 = PRODUCT_RELATED_PRODUCT_CATEGORY ( 'detail', '', ( #3194 ) ) ;
#13798 = MANIFOLD_SOLID_BREP ( 'SOLID22[1]', #22930 ) ;
#13799 = CARTESIAN_POINT ( 'NONE',  ( 136.8551930556999991, -3659.717490576542787, 2250.213681781542618 ) ) ;
#13800 = CARTESIAN_POINT ( 'NONE',  ( 14.61266695128000137, -3657.399152860999493, 2246.630000000000109 ) ) ;
#13801 = LINE ( 'NONE', #18830, #14327 ) ;
#13802 = ORIENTED_EDGE ( 'NONE', *, *, #2823, .F. ) ;
#13803 = ORIENTED_EDGE ( 'NONE', *, *, #7301, .T. ) ;
#13804 = EDGE_CURVE ( 'NONE', #18172, #17044, #8449, .T. ) ;
#13805 = VERTEX_POINT ( 'NONE', #7173 ) ;
#13806 = CARTESIAN_POINT ( 'NONE',  ( 10.21049783562838265, -3600.934814744884534, 2296.591799999930117 ) ) ;
#13807 = EDGE_CURVE ( 'NONE', #16242, #2028, #11424, .T. ) ;
#13808 = ORIENTED_EDGE ( 'NONE', *, *, #55, .F. ) ;
#13809 = CARTESIAN_POINT ( 'NONE',  ( 14.50480255619999959, -3581.700066511000387, 2257.739429448999999 ) ) ;
#13810 = APPROVAL_ROLE ( '' ) ;
#13811 = EDGE_CURVE ( 'NONE', #22211, #9308, #14438, .T. ) ;
#13812 = DIRECTION ( 'NONE',  ( 0.000000000000000000, -1.000000000000000000, 0.000000000000000000 ) ) ;
#13813 = CARTESIAN_POINT ( 'NONE',  ( 12.70000000000000107, -3648.710000000000036, 2279.817639999999756 ) ) ;
#13814 = FACE_OUTER_BOUND ( 'NONE', #1602, .T. ) ;
#13815 = CIRCLE ( 'NONE', #3312, 5.460999999999938126 ) ;
#13816 = CARTESIAN_POINT ( 'NONE',  ( 14.90546723228000126, -3657.700681481000174, 2257.813182709000102 ) ) ;
#13817 = CARTESIAN_POINT ( 'NONE',  ( 139.6999999999999886, -3579.494999999999891, 2239.391000000000076 ) ) ;
#13818 = ADVANCED_FACE ( 'NONE', ( #17066 ), #11798, .T. ) ;
#13819 = LINE ( 'NONE', #5150, #16611 ) ;
#13820 = ORIENTED_EDGE ( 'NONE', *, *, #14557, .F. ) ;
#13821 = DIRECTION ( 'NONE',  ( 0.000000000000000000, 0.000000000000000000, -1.000000000000000000 ) ) ;
#13822 = CARTESIAN_POINT ( 'NONE',  ( 101.5999999999999943, -3670.300000000000182, 2259.837999999999738 ) ) ;
#13823 = VERTEX_POINT ( 'NONE', #18951 ) ;
#13824 = EDGE_CURVE ( 'NONE', #22778, #6851, #11919, .T. ) ;
#13825 = DIRECTION ( 'NONE',  ( -1.000000000000000000, 0.000000000000000000, 0.000000000000000000 ) ) ;
#13826 = CARTESIAN_POINT ( 'NONE',  ( 151.1299999999999955, -3578.860000000000127, 2250.236800000000130 ) ) ;
#13827 = ORIENTED_EDGE ( 'NONE', *, *, #4223, .F. ) ;
#13828 = ORIENTED_EDGE ( 'NONE', *, *, #16650, .T. ) ;
#13829 = DIRECTION ( 'NONE',  ( -2.824627736850999825E-12, 1.000000000000000000, 0.000000000000000000 ) ) ;
#13830 = ORIENTED_EDGE ( 'NONE', *, *, #20706, .F. ) ;
#13831 = DIRECTION ( 'NONE',  ( -1.000000000000000000, 0.000000000000000000, 0.000000000000000000 ) ) ;
#13832 = CARTESIAN_POINT ( 'NONE',  ( 21.19471181662999726, -3544.570000000000164, 2259.679250718999810 ) ) ;
#13833 = ORIENTED_EDGE ( 'NONE', *, *, #17603, .T. ) ;
#13834 = PLANE ( 'NONE',  #17110 ) ;
#13835 = ADVANCED_FACE ( 'NONE', ( #17182 ), #4111, .F. ) ;
#13836 = APPROVAL_STATUS ( 'not_yet_approved' ) ;
#13837 = EDGE_CURVE ( 'NONE', #22778, #13538, #13199, .T. ) ;
#13838 = DIRECTION ( 'NONE',  ( -0.000000000000000000, 1.000000000000000000, 0.000000000000000000 ) ) ;
#13839 = FACE_OUTER_BOUND ( 'NONE', #19374, .T. ) ;
#13840 = AXIS2_PLACEMENT_3D ( 'NONE', #21449, #5397, #14419 ) ;
#13841 = CARTESIAN_POINT ( 'NONE',  ( 134.1558484328602390, -3658.117549335799595, 2245.390303089542158 ) ) ;
#13842 = LOCAL_TIME ( 17, 37, 43.00000000000000000, #18993 ) ;
#13843 = CARTESIAN_POINT ( 'NONE',  ( 12.69999999999999929, -3653.027999999999793, 2275.055139999999483 ) ) ;
#13844 = EDGE_LOOP ( 'NONE', ( #19310, #18053, #12081, #19639 ) ) ;
#13845 = CIRCLE ( 'NONE', #363, 0.7619999999999294005 ) ;
#13846 = CARTESIAN_POINT ( 'NONE',  ( 15.66246403760665196, -3695.684982104464325, 2254.716693470072187 ) ) ;
#13847 = ORIENTED_EDGE ( 'NONE', *, *, #14140, .T. ) ;
#13848 = CYLINDRICAL_SURFACE ( 'NONE', #18823, 2.844800000000091700 ) ;
#13849 = CARTESIAN_POINT ( 'NONE',  ( 15.54479999999999862, -3579.494999999999891, 2256.063560000000052 ) ) ;
#13850 = VERTEX_POINT ( 'NONE', #8176 ) ;
#13851 = VERTEX_POINT ( 'NONE', #11256 ) ;
#13852 = DIRECTION ( 'NONE',  ( 0.000000000000000000, 0.000000000000000000, -1.000000000000000000 ) ) ;
#13853 = PLANE ( 'NONE',  #11792 ) ;
#13854 = ORIENTED_EDGE ( 'NONE', *, *, #16885, .F. ) ;
#13855 = FACE_OUTER_BOUND ( 'NONE', #4007, .T. ) ;
#13856 = CARTESIAN_POINT ( 'NONE',  ( 135.5205281809360827, -3657.399153614157967, 2246.629997290541269 ) ) ;
#13857 = DIRECTION ( 'NONE',  ( -2.324635735433000053E-14, 2.336881798971000105E-14, -1.000000000000000000 ) ) ;
#13858 = APPLIED_APPROVAL_ASSIGNMENT ( #5631, ( #5262 ) ) ;
#13859 =( GEOMETRIC_REPRESENTATION_CONTEXT ( 3 ) GLOBAL_UNCERTAINTY_ASSIGNED_CONTEXT ( ( #4088 ) ) GLOBAL_UNIT_ASSIGNED_CONTEXT ( ( #16644, #4115, #9166 ) ) REPRESENTATION_CONTEXT ( 'NONE', 'WORKASPACE' ) );
#13860 = CARTESIAN_POINT ( 'NONE',  ( 50.79999999999999716, -3619.500000000000000, 2239.009999999999764 ) ) ;
#13861 = APPROVAL_DATE_TIME ( #22633, #17646 ) ;
#13862 = DIRECTION ( 'NONE',  ( 0.000000000000000000, 0.000000000000000000, -1.000000000000000000 ) ) ;
#13863 = DIRECTION ( 'NONE',  ( -1.000000000000000000, 0.000000000000000000, 0.000000000000000000 ) ) ;
#13864 = DIRECTION ( 'NONE',  ( -1.000000000000000000, 0.000000000000000000, 1.295098308114000000E-13 ) ) ;
#13865 = B_SPLINE_CURVE_WITH_KNOTS ( 'NONE', 3,
 ( #316, #12623, #10745, #19530 ),
 .UNSPECIFIED., .F., .F.,
 ( 4, 4 ),
 ( 0.000000000000000000, 1.000000000000000000 ),
 .UNSPECIFIED. ) ;
#13866 = EDGE_CURVE ( 'NONE', #3802, #13513, #18402, .T. ) ;
#13867 = CARTESIAN_POINT ( 'NONE',  ( 142.1532463573187215, -3658.064754788580103, 2249.338046269550887 ) ) ;
#13868 = EDGE_CURVE ( 'NONE', #20725, #16084, #10539, .T. ) ;
#13869 = EDGE_CURVE ( 'NONE', #10418, #7999, #3565, .T. ) ;
#13870 = ORIENTED_EDGE ( 'NONE', *, *, #4840, .F. ) ;
#13871 = DIRECTION ( 'NONE',  ( -1.000000000000000000, 0.000000000000000000, 0.000000000000000000 ) ) ;
#13872 = ORIENTED_EDGE ( 'NONE', *, *, #18195, .F. ) ;
#13873 = ORGANIZATION ( 'NAUO-ORG5', 'UNSPECIFIED', 'UNSPECIFIED' ) ;
#13874 = EDGE_CURVE ( 'NONE', #12370, #2712, #19568, .T. ) ;
#13875 = APPLIED_SECURITY_CLASSIFICATION_ASSIGNMENT ( #4495, ( #16119 ) ) ;
#13876 = ORIENTED_EDGE ( 'NONE', *, *, #15138, .F. ) ;
#13877 = DIRECTION ( 'NONE',  ( 0.000000000000000000, 0.000000000000000000, 1.000000000000000000 ) ) ;
#13878 = VERTEX_POINT ( 'NONE', #4533 ) ;
#13879 = ORIENTED_EDGE ( 'NONE', *, *, #22811, .F. ) ;
#13880 = DIRECTION ( 'NONE',  ( 0.000000000000000000, 0.000000000000000000, 1.000000000000000000 ) ) ;
#13881 = CARTESIAN_POINT ( 'NONE',  ( 12.70000000000000107, -3648.710000000000036, 2279.817639999999756 ) ) ;
#13882 = CARTESIAN_POINT ( 'NONE',  ( 12.69999999999999929, -3590.289999999999964, 2257.592639999999847 ) ) ;
#13883 = EDGE_CURVE ( 'NONE', #6665, #5168, #2724, .T. ) ;
#13884 = EDGE_LOOP ( 'NONE', ( #10045, #16916, #22106, #7434 ) ) ;
#13885 = AXIS2_PLACEMENT_3D ( 'NONE', #8148, #8257, #22534 ) ;
#13886 = CARTESIAN_POINT ( 'NONE',  ( 57.14999999999999858, -3694.430000000000291, 2244.547199999999975 ) ) ;
#13887 = EDGE_CURVE ( 'NONE', #17007, #5186, #4883, .T. ) ;
#13888 = DIRECTION ( 'NONE',  ( 2.324635735433000053E-14, 0.000000000000000000, 1.000000000000000000 ) ) ;
#13889 = CARTESIAN_POINT ( 'NONE',  ( 101.5999999999999943, -3619.500000000000000, 2239.771999999999935 ) ) ;
#13890 = CARTESIAN_POINT ( 'NONE',  ( 138.7804567414061410, -3656.806478193061594, 2257.629402112182561 ) ) ;
#13891 = FACE_OUTER_BOUND ( 'NONE', #15307, .T. ) ;
#13892 = ORIENTED_EDGE ( 'NONE', *, *, #17383, .T. ) ;
#13893 = PRODUCT_CONTEXT ( 'NONE', #12012, 'mechanical' ) ;
#13894 = ORIENTED_EDGE ( 'NONE', *, *, #5272, .T. ) ;
#13895 = DIRECTION ( 'NONE',  ( 0.000000000000000000, 0.000000000000000000, -1.000000000000000000 ) ) ;
#13896 = ORGANIZATION ( 'NAUO-ORG14', 'UNSPECIFIED', 'UNSPECIFIED' ) ;
#13897 = DIRECTION ( 'NONE',  ( 0.000000000000000000, 0.000000000000000000, -1.000000000000000000 ) ) ;
#13898 = ORIENTED_EDGE ( 'NONE', *, *, #20460, .F. ) ;
#13899 = DIRECTION ( 'NONE',  ( 0.000000000000000000, 1.000000000000000000, 0.000000000000000000 ) ) ;
#13900 = VERTEX_POINT ( 'NONE', #15674 ) ;
#13901 = AXIS2_PLACEMENT_3D ( 'NONE', #9343, #19892, #18126 ) ;
#13902 = FACE_BOUND ( 'NONE', #19378, .T. ) ;
#13903 = VECTOR ( 'NONE', #9641, 1000.000000000000000 ) ;
#13904 = CARTESIAN_POINT ( 'NONE',  ( 29.00679999999900005, -3670.300000000000182, 2239.771999999999935 ) ) ;
#13905 = CARTESIAN_POINT ( 'NONE',  ( 144.4335724592128258, -3662.708189880353530, 2246.166055327533286 ) ) ;
#13906 = DIRECTION ( 'NONE',  ( -1.000000000000000000, 0.000000000000000000, 0.000000000000000000 ) ) ;
#13907 = CARTESIAN_POINT ( 'NONE',  ( 10.99177528568289830, -3661.779950359641589, 2249.716450903262285 ) ) ;
#13908 = CARTESIAN_POINT ( 'NONE',  ( 147.4191137077191627, -3543.814512432531501, 2260.351687526631849 ) ) ;
#13909 = ORIENTED_EDGE ( 'NONE', *, *, #8136, .F. ) ;
#13910 = CARTESIAN_POINT ( 'NONE',  ( -8.890000000004999237, -3662.832400000000234, 2247.392000000000280 ) ) ;
#13911 = DIRECTION ( 'NONE',  ( 2.330758767201999921E-14, 1.000000000000000000, 0.000000000000000000 ) ) ;
#13912 = DIRECTION ( 'NONE',  ( 0.000000000000000000, 1.000000000000000000, 0.000000000000000000 ) ) ;
#13913 = DIRECTION ( 'NONE',  ( 0.000000000000000000, -1.000000000000000000, 0.000000000000000000 ) ) ;
#13914 = FACE_OUTER_BOUND ( 'NONE', #20705, .T. ) ;
#13915 = ORIENTED_EDGE ( 'NONE', *, *, #9245, .F. ) ;
#13916 = TOROIDAL_SURFACE ( 'NONE', #18410, 3.606799999999999784, 0.7620000000000000107 ) ;
#13917 = ORIENTED_EDGE ( 'NONE', *, *, #3504, .T. ) ;
#13918 = AXIS2_PLACEMENT_3D ( 'NONE', #15588, #22723, #15701 ) ;
#13919 = DIRECTION ( 'NONE',  ( 0.000000000000000000, 0.000000000000000000, 1.000000000000000000 ) ) ;
#13920 = VERTEX_POINT ( 'NONE', #22798 ) ;
#13921 = CARTESIAN_POINT ( 'NONE',  ( 9.737535961660340078, -3543.315017895228266, 2254.716693468255016 ) ) ;
#13922 = APPROVAL_STATUS ( 'not_yet_approved' ) ;
#13923 = CARTESIAN_POINT ( 'NONE',  ( 134.3871257472000025, -3657.399152860999493, 2246.630000000000109 ) ) ;
#13924 = CARTESIAN_POINT ( 'NONE',  ( 11.61864837389999927, -3656.868790608999916, 2257.644359388999874 ) ) ;
#13925 = CARTESIAN_POINT ( 'NONE',  ( 10.06338274650999942, -3660.585356121999666, 2257.909778189000008 ) ) ;
#13926 = AXIS2_PLACEMENT_3D ( 'NONE', #6175, #4516, #8162 ) ;
#13927 = CARTESIAN_POINT ( 'NONE',  ( 14.71514678359000072, -3657.490332083999874, 2257.776246897999954 ) ) ;
#13928 = APPROVAL ( #4204, 'UNSPECIFIED' ) ;
#13929 = DIRECTION ( 'NONE',  ( -0.8660254037817188832, 0.5000000000047110094, 3.181634500920069822E-14 ) ) ;
#13930 = AXIS2_PLACEMENT_3D ( 'NONE', #18609, #11341, #8180 ) ;
#13931 = DIRECTION ( 'NONE',  ( 0.000000000000000000, 0.000000000000000000, -1.000000000000000000 ) ) ;
#13932 = ORIENTED_EDGE ( 'NONE', *, *, #13378, .T. ) ;
#13933 = CIRCLE ( 'NONE', #19554, 0.7619999999999987894 ) ;
#13934 = CARTESIAN_POINT ( 'NONE',  ( 136.9873132028999976, -3661.071170452878050, 2239.009999999999764 ) ) ;
#13935 = VECTOR ( 'NONE', #11673, 1000.000000000000000 ) ;
#13936 = EDGE_CURVE ( 'NONE', #6119, #15991, #21809, .T. ) ;
#13937 = CARTESIAN_POINT ( 'NONE',  ( 15.87500000000000000, -3694.938000000000102, 2281.351799999999912 ) ) ;
#13938 = ORIENTED_EDGE ( 'NONE', *, *, #8593, .F. ) ;
#13939 = CARTESIAN_POINT ( 'NONE',  ( 9.926995637850000165, -3660.140002548000211, 2250.236801297000056 ) ) ;
#13940 = CARTESIAN_POINT ( 'NONE',  ( 10.80609603922892070, -3657.382216624303055, 2248.090589125378301 ) ) ;
#13941 = EDGE_CURVE ( 'NONE', #14116, #15892, #3244, .T. ) ;
#13942 = EDGE_LOOP ( 'NONE', ( #596, #1072, #21481, #397 ) ) ;
#13943 = CARTESIAN_POINT ( 'NONE',  ( 132.2768405780999785, -3694.472271328999796, 2260.413001451000127 ) ) ;
#13944 = CIRCLE ( 'NONE', #16919, 0.7619999999999294005 ) ;
#13945 = ORIENTED_EDGE ( 'NONE', *, *, #19024, .F. ) ;
#13946 = FACE_BOUND ( 'NONE', #1558, .T. ) ;
#13947 = DATE_AND_TIME ( #17451, #10884 ) ;
#13948 = DIRECTION ( 'NONE',  ( -0.7249994335944509594, 0.000000000000000000, 0.6887494619146539154 ) ) ;
#13949 = ORIENTED_EDGE ( 'NONE', *, *, #18548, .F. ) ;
#13950 = CARTESIAN_POINT ( 'NONE',  ( 131.7385023306979406, -3695.630398139015142, 2259.744659233807397 ) ) ;
#13951 = COORDINATED_UNIVERSAL_TIME_OFFSET ( 0, 0, .AHEAD. ) ;
#13952 = AXIS2_PLACEMENT_3D ( 'NONE', #5301, #20891, #1306 ) ;
#13953 = CARTESIAN_POINT ( 'NONE',  ( -6.730999999999999872, -3578.860000000000127, 2247.392000000000280 ) ) ;
#13954 = CARTESIAN_POINT ( 'NONE',  ( 15.11849031972590041, -3580.993088984551378, 2249.274435424331841 ) ) ;
#13955 = CARTESIAN_POINT ( 'NONE',  ( 134.0922626992376081, -3658.402569313454933, 2245.138333345573756 ) ) ;
#13956 = DIRECTION ( 'NONE',  ( 0.000000000000000000, 0.000000000000000000, 1.000000000000000000 ) ) ;
#13957 = ORIENTED_EDGE ( 'NONE', *, *, #22733, .T. ) ;
#13958 = AXIS2_PLACEMENT_3D ( 'NONE', #13225, #7845, #20159 ) ;
#13959 = CARTESIAN_POINT ( 'NONE',  ( 142.2400000000000091, -3544.570000000000164, 2255.774000000000342 ) ) ;
#13960 = EDGE_CURVE ( 'NONE', #20359, #13759, #12827, .T. ) ;
#13961 = CARTESIAN_POINT ( 'NONE',  ( 0.7620000000000000107, -3694.938000000000102, 2239.009999999999764 ) ) ;
#13962 = ORIENTED_EDGE ( 'NONE', *, *, #20878, .T. ) ;
#13963 = ADVANCED_FACE ( 'NONE', ( #317 ), #3098, .T. ) ;
#13964 = FACE_OUTER_BOUND ( 'NONE', #2920, .T. ) ;
#13965 = AXIS2_PLACEMENT_3D ( 'NONE', #17481, #5070, #22631 ) ;
#13966 = EDGE_CURVE ( 'NONE', #7066, #19732, #216, .T. ) ;
#13967 = ADVANCED_FACE ( 'NONE', ( #10974 ), #10207, .T. ) ;
#13968 = CIRCLE ( 'NONE', #19571, 5.080000000000000959 ) ;
#13969 = DIRECTION ( 'NONE',  ( 1.298916404569000195E-12, -1.000000000000000000, 0.000000000000000000 ) ) ;
#13970 = EDGE_LOOP ( 'NONE', ( #7750, #11156, #17850, #17084 ) ) ;
#13971 = VERTEX_POINT ( 'NONE', #2414 ) ;
#13972 = DIRECTION ( 'NONE',  ( 0.000000000000000000, 0.000000000000000000, -1.000000000000000000 ) ) ;
#13973 = CARTESIAN_POINT ( 'NONE',  ( 12.69999999999999929, -3577.590000000000146, 2272.030000000000200 ) ) ;
#13974 = EDGE_LOOP ( 'NONE', ( #10257, #11443 ) ) ;
#13975 = FACE_BOUND ( 'NONE', #20336, .T. ) ;
#13976 = CARTESIAN_POINT ( 'NONE',  ( 15.52082456645615238, -3659.877973396570724, 2250.225202194340000 ) ) ;
#13977 = LINE ( 'NONE', #22981, #18588 ) ;
#13978 = CIRCLE ( 'NONE', #3868, 0.7619999999999294005 ) ;
#13979 = COORDINATED_UNIVERSAL_TIME_OFFSET ( 0, 0, .AHEAD. ) ;
#13980 = AXIS2_PLACEMENT_3D ( 'NONE', #8762, #18988, #13474 ) ;
#13981 = CARTESIAN_POINT ( 'NONE',  ( 6.985153502415999860, -3659.505556594000154, 2244.618656866000038 ) ) ;
#13982 = DIRECTION ( 'NONE',  ( -1.000000000000000000, 0.000000000000000000, 0.000000000000000000 ) ) ;
#13983 = CARTESIAN_POINT ( 'NONE',  ( 18.37871628331206608, -3580.137931053087868, 2244.850299910469857 ) ) ;
#13984 = EDGE_CURVE ( 'NONE', #6446, #11488, #9087, .T. ) ;
#13985 = TOROIDAL_SURFACE ( 'NONE', #10566, 1.905000000000000027, 1.270000000000000018 ) ;
#13986 = CLOSED_SHELL ( 'NONE', ( #4907, #11558, #20122, #16856, #14732, #14967, #11164, #2412, #2656, #12456, #14296, #14448, #21825, #8111, #3348, #19672, #10253, #13818, #8711, #23104, #2093, #10859, #2347, #9367, #7725, #4390 ) ) ;
#13987 = CARTESIAN_POINT ( 'NONE',  ( 141.4997331193342518, -3657.301708037173285, 2247.198575533412622 ) ) ;
#13988 = VERTEX_POINT ( 'NONE', #14502 ) ;
#13989 = DIRECTION ( 'NONE',  ( 0.000000000000000000, 1.000000000000000000, 0.000000000000000000 ) ) ;
#13990 = MANIFOLD_SOLID_BREP ( 'TORNILLO2[1]', #13986 ) ;
#13991 = ORIENTED_EDGE ( 'NONE', *, *, #16709, .F. ) ;
#13992 = ORIENTED_EDGE ( 'NONE', *, *, #3070, .F. ) ;
#13993 = VERTEX_POINT ( 'NONE', #16364 ) ;
#13994 = CIRCLE ( 'NONE', #18832, 2.844800000000091700 ) ;
#13995 = EDGE_CURVE ( 'NONE', #6733, #4557, #11746, .T. ) ;
#13996 = CARTESIAN_POINT ( 'NONE',  ( 15.03168679716000078, -3578.148799999999937, 2242.820000000000164 ) ) ;
#13997 = VERTEX_POINT ( 'NONE', #11095 ) ;
#13998 = ORIENTED_EDGE ( 'NONE', *, *, #16267, .F. ) ;
#13999 = CARTESIAN_POINT ( 'NONE',  ( 4.618254035402077129, -3543.300000000021555, 2259.443539528608198 ) ) ;
#14000 = DATE_AND_TIME ( #168, #2639 ) ;
#14001 = DIRECTION ( 'NONE',  ( 1.000000000000000000, 0.000000000000000000, 0.000000000000000000 ) ) ;
#14002 = LINE ( 'NONE', #5215, #20436 ) ;
#14003 = ADVANCED_FACE ( 'NONE', ( #9338 ), #539, .F. ) ;
#14004 = ORIENTED_EDGE ( 'NONE', *, *, #16436, .F. ) ;
#14005 = EDGE_CURVE ( 'NONE', #15820, #6172, #22967, .T. ) ;
#14006 = CARTESIAN_POINT ( 'NONE',  ( 138.3436566013999993, -3661.854255679000289, 2239.391000000000076 ) ) ;
#14007 = FACE_BOUND ( 'NONE', #11326, .T. ) ;
#14008 = DIRECTION ( 'NONE',  ( 0.000000000000000000, 1.000000000000000000, 0.000000000000000000 ) ) ;
#14009 = DIRECTION ( 'NONE',  ( 1.000000000000000000, 0.000000000000000000, 0.000000000000000000 ) ) ;
#14010 = ORIENTED_EDGE ( 'NONE', *, *, #11854, .F. ) ;
#14011 = COORDINATED_UNIVERSAL_TIME_OFFSET ( 0, 0, .AHEAD. ) ;
#14012 = ORIENTED_EDGE ( 'NONE', *, *, #14688, .T. ) ;
#14013 = EDGE_CURVE ( 'NONE', #650, #9827, #2302, .T. ) ;
#14014 = AXIS2_PLACEMENT_3D ( 'NONE', #10408, #10293, #7030 ) ;
#14015 = CARTESIAN_POINT ( 'NONE',  ( 10.13694260842256689, -3580.732079930104646, 2249.536708023868414 ) ) ;
#14016 = CARTESIAN_POINT ( 'NONE',  ( 0.7620000000000000107, -3544.061999999999898, 2295.829799999999977 ) ) ;
#14017 = CIRCLE ( 'NONE', #15134, 3.606800000000000228 ) ;
#14018 = ORIENTED_EDGE ( 'NONE', *, *, #10587, .T. ) ;
#14019 = EDGE_CURVE ( 'NONE', #7868, #19336, #15295, .T. ) ;
#14020 = DIRECTION ( 'NONE',  ( 0.000000000000000000, 0.000000000000000000, 1.000000000000000000 ) ) ;
#14021 = EDGE_CURVE ( 'NONE', #23163, #2067, #6287, .T. ) ;
#14022 = CARTESIAN_POINT ( 'NONE',  ( 12.69999999999999929, -3570.287499999999909, 2268.705139999999574 ) ) ;
#14023 = DIRECTION ( 'NONE',  ( 0.000000000000000000, 0.000000000000000000, -1.000000000000000000 ) ) ;
#14024 = CARTESIAN_POINT ( 'NONE',  ( 12.83072102879435405, -3662.349731445673115, 2249.183616308214823 ) ) ;
#14025 = DIRECTION ( 'NONE',  ( 0.8660254037826368156, 0.5000000000031208369, 0.000000000000000000 ) ) ;
#14026 = ORIENTED_EDGE ( 'NONE', *, *, #13936, .F. ) ;
#14027 = LINE ( 'NONE', #10268, #2034 ) ;
#14028 = CIRCLE ( 'NONE', #179, 3.606799999999001027 ) ;
#14029 = CARTESIAN_POINT ( 'NONE',  ( 76.20000000000000284, -3568.700000000000273, 2259.837999999999738 ) ) ;
#14030 = CIRCLE ( 'NONE', #16269, 5.460999999999938126 ) ;
#14031 = EDGE_CURVE ( 'NONE', #3687, #7518, #8262, .T. ) ;
#14032 = CARTESIAN_POINT ( 'NONE',  ( 98.75520000000000209, -3619.500000000000000, 2259.837999999999738 ) ) ;
#14033 = CIRCLE ( 'NONE', #8427, 3.606800000000021100 ) ;
#14034 = CARTESIAN_POINT ( 'NONE',  ( 15.14452126063228832, -3658.050008149689802, 2249.322202696583190 ) ) ;
#14035 = CARTESIAN_POINT ( 'NONE',  ( 15.47299515201000020, -3578.859991782000179, 2250.236800948000109 ) ) ;
#14036 = ORIENTED_EDGE ( 'NONE', *, *, #3640, .T. ) ;
#14037 = ORIENTED_EDGE ( 'NONE', *, *, #19751, .F. ) ;
#14038 = PLANE ( 'NONE',  #17293 ) ;
#14039 = CARTESIAN_POINT ( 'NONE',  ( 9.822867848221497056, -3543.373434452745187, 2254.929970520540337 ) ) ;
#14040 = CONTEXT_DEPENDENT_SHAPE_REPRESENTATION ( #10083, #7907 ) ;
#14041 = CYLINDRICAL_SURFACE ( 'NONE', #5340, 0.7620000000000001217 ) ;
#14042 = DIRECTION ( 'NONE',  ( -1.000000000000000000, 0.000000000000000000, 0.000000000000000000 ) ) ;
#14043 = CARTESIAN_POINT ( 'NONE',  ( 12.60780787143999859, -3662.349800030000097, 2257.592639999999847 ) ) ;
#14044 = TOROIDAL_SURFACE ( 'NONE', #5452, 6.477000000000000313, 0.7620000000000000107 ) ;
#14045 = AXIS2_PLACEMENT_3D ( 'NONE', #20437, #4387, #11526 ) ;
#14046 = EDGE_CURVE ( 'NONE', #7103, #17227, #8298, .T. ) ;
#14047 = FACE_OUTER_BOUND ( 'NONE', #6274, .T. ) ;
#14048 = VECTOR ( 'NONE', #20966, 1000.000000000000000 ) ;
#14049 = CARTESIAN_POINT ( 'NONE',  ( 18.16100000000000136, -3639.502500000000055, 2290.622800000000097 ) ) ;
#14050 = AXIS2_PLACEMENT_3D ( 'NONE', #4139, #18431, #20312 ) ;
#14051 = FACE_OUTER_BOUND ( 'NONE', #5923, .T. ) ;
#14052 = ORIENTED_EDGE ( 'NONE', *, *, #7835, .F. ) ;
#14053 = DIRECTION ( 'NONE',  ( -2.330758767202000237E-14, -1.000000000000000000, -1.224646799141892318E-16 ) ) ;
#14054 = CYLINDRICAL_SURFACE ( 'NONE', #19662, 5.460999999999938126 ) ;
#14055 = ORIENTED_EDGE ( 'NONE', *, *, #691, .T. ) ;
#14056 = LINE ( 'NONE', #17441, #21904 ) ;
#14057 = VERTEX_POINT ( 'NONE', #20554 ) ;
#14058 = CARTESIAN_POINT ( 'NONE',  ( 133.9850000019999925, -3579.494756921999851, 2244.617465693000213 ) ) ;
#14059 = VECTOR ( 'NONE', #8777, 1000.000000000000114 ) ;
#14060 = ORIENTED_EDGE ( 'NONE', *, *, #12927, .T. ) ;
#14061 = EDGE_LOOP ( 'NONE', ( #17119, #13854, #5622, #22044 ) ) ;
#14062 = APPROVAL ( #14234, 'UNKNOWN' ) ;
#14063 = DIRECTION ( 'NONE',  ( 1.000000000000000000, 5.432398939370942693E-28, -2.324635735433000053E-14 ) ) ;
#14064 = CALENDAR_DATE ( 2026, 26, 10 ) ;
#14065 = AXIS2_PLACEMENT_3D ( 'NONE', #12521, #5383, #21776 ) ;
#14066 = DIRECTION ( 'NONE',  ( 0.000000000000000000, 0.000000000000000000, -1.000000000000000000 ) ) ;
#14067 = ORIENTED_EDGE ( 'NONE', *, *, #16236, .T. ) ;
#14068 = CARTESIAN_POINT ( 'NONE',  ( 131.9781484670521081, -3695.197007937890248, 2260.344194844531557 ) ) ;
#14069 = AXIS2_PLACEMENT_3D ( 'NONE', #253, #18699, #2649 ) ;
#14070 = DATE_AND_TIME ( #12311, #7886 ) ;
#14071 = CARTESIAN_POINT ( 'NONE',  ( 139.6999999999999886, -3570.287499999999909, 2268.705139999999574 ) ) ;
#14072 = CARTESIAN_POINT ( 'NONE',  ( 15.35230487608980710, -3580.523739450907669, 2249.699608343330965 ) ) ;
#14073 = CARTESIAN_POINT ( 'NONE',  ( 134.6199999999999761, -3659.504999999999654, 2239.391000000000076 ) ) ;
#14074 = DIRECTION ( 'NONE',  ( -1.000000000000000000, -1.295098308114000000E-13, 0.000000000000000000 ) ) ;
#14075 = AXIS2_PLACEMENT_3D ( 'NONE', #19390, #21032, #10360 ) ;
#14076 = DIRECTION ( 'NONE',  ( 0.000000000000000000, 0.000000000000000000, 1.000000000000000000 ) ) ;
#14077 = ORIENTED_EDGE ( 'NONE', *, *, #4542, .F. ) ;
#14078 = AXIS2_PLACEMENT_3D ( 'NONE', #5236, #21179, #23140 ) ;
#14079 = CARTESIAN_POINT ( 'NONE',  ( 15.57713215129027340, -3695.626565546841903, 2254.929970521695395 ) ) ;
#14080 = VECTOR ( 'NONE', #3601, 1000.000000000000000 ) ;
#14081 = EDGE_LOOP ( 'NONE', ( #5566, #19535, #7304 ) ) ;
#14082 = CARTESIAN_POINT ( 'NONE',  ( 28.24479999999899604, -3670.300000000000182, 2239.771999999999935 ) ) ;
#14083 = AXIS2_PLACEMENT_3D ( 'NONE', #12261, #19406, #3340 ) ;
#14084 = CARTESIAN_POINT ( 'NONE',  ( 15.41268679717000012, -3659.504999999999654, 2239.391000000000076 ) ) ;
#14085 = AXIS2_PLACEMENT_3D ( 'NONE', #15352, #16642, #16869 ) ;
#14086 = EDGE_LOOP ( 'NONE', ( #11460, #4780, #9332, #3445, #11386, #11483 ) ) ;
#14087 = CIRCLE ( 'NONE', #9957, 0.7619999999999294005 ) ;
#14088 = ORIENTED_EDGE ( 'NONE', *, *, #4996, .T. ) ;
#14089 = LINE ( 'NONE', #17347, #16161 ) ;
#14090 = FACE_OUTER_BOUND ( 'NONE', #11966, .T. ) ;
#14091 = EDGE_LOOP ( 'NONE', ( #9158, #12014 ) ) ;
#14092 = APPLIED_PERSON_AND_ORGANIZATION_ASSIGNMENT ( #3826, #5604, ( #14623 ) ) ;
#14093 = CARTESIAN_POINT ( 'NONE',  ( 12.70000000003999929, -3582.627340905000437, 2239.009999999999764 ) ) ;
#14094 = CARTESIAN_POINT ( 'NONE',  ( 0.000000000000000000, -3578.860000000000127, 2247.392000000000280 ) ) ;
#14095 = CARTESIAN_POINT ( 'NONE',  ( 14.47433926966999884, -3601.728985385999749, 2279.676072425999791 ) ) ;
#14096 = CARTESIAN_POINT ( 'NONE',  ( 0.000000000000000000, -3544.061999999999898, 2239.771999999999935 ) ) ;
#14097 = PERSON_AND_ORGANIZATION ( #5446, #1895 ) ;
#14098 = EDGE_CURVE ( 'NONE', #7086, #22455, #12460, .T. ) ;
#14099 = DIRECTION ( 'NONE',  ( 0.5000000000047110094, -0.8660254037817188832, 0.000000000000000000 ) ) ;
#14100 = CARTESIAN_POINT ( 'NONE',  ( 10.01415227263506580, -3695.321318630586120, 2255.408757311871341 ) ) ;
#14102 = ADVANCED_FACE ( 'NONE', ( #2529 ), #9672, .F. ) ;
#14101 = CARTESIAN_POINT ( 'NONE',  ( 25.39999999999999858, -3568.700000000000273, 2261.869999999999891 ) ) ;
#14103 = AXIS2_PLACEMENT_3D ( 'NONE', #22527, #6497, #22296 ) ;
#14104 = EDGE_CURVE ( 'NONE', #15061, #185, #13184, .T. ) ;
#14105 = CARTESIAN_POINT ( 'NONE',  ( 137.3103389895218243, -3657.961604733812692, 2249.221652488155087 ) ) ;
#14106 = ORIENTED_EDGE ( 'NONE', *, *, #6648, .F. ) ;
#14107 = LINE ( 'NONE', #5315, #1358 ) ;
#14108 = VERTEX_POINT ( 'NONE', #19043 ) ;
#14109 = ADVANCED_FACE ( 'NONE', ( #18799 ), #4960, .T. ) ;
#14110 = VERTEX_POINT ( 'NONE', #6165 ) ;
#14111 = ORIENTED_EDGE ( 'NONE', *, *, #3935, .T. ) ;
#14112 = CIRCLE ( 'NONE', #15280, 2.844800000000091700 ) ;
#14113 = TOROIDAL_SURFACE ( 'NONE', #21596, 4.114799999999999791, 1.270000000000000018 ) ;
#14114 = CARTESIAN_POINT ( 'NONE',  ( 18.41499999999899728, -3599.497499999999945, 2288.971800000000258 ) ) ;
#14115 = VERTEX_POINT ( 'NONE', #8032 ) ;
#14116 = VERTEX_POINT ( 'NONE', #4402 ) ;
#14117 = CARTESIAN_POINT ( 'NONE',  ( 4.572920519510000226, -3543.299999999999727, 2259.329999999999927 ) ) ;
#14118 = EDGE_CURVE ( 'NONE', #5536, #13127, #14707, .T. ) ;
#14119 = APPROVAL_STATUS ( 'not_yet_approved' ) ;
#14120 = CARTESIAN_POINT ( 'NONE',  ( 12.69999999999999929, -3601.402499999999691, 2264.841800000000148 ) ) ;
#14121 = PERSON ( 'NAUO-PER13', 'UNSPECIFIED', 'UNSPECIFIED', ('UNSPECIFIED'), ('UNSPECIFIED'), ('UNSPECIFIED') ) ;
#14122 = CIRCLE ( 'NONE', #7020, 0.7619999999999987894 ) ;
#14123 = DIRECTION ( 'NONE',  ( 0.000000000000000000, 0.000000000000000000, -1.000000000000000000 ) ) ;
#14124 = ORIENTED_EDGE ( 'NONE', *, *, #20185, .T. ) ;
#14125 = CARTESIAN_POINT ( 'NONE',  ( 3.048000000000000043, -3694.938000000000102, 2238.248000000000047 ) ) ;
#14126 = DIRECTION ( 'NONE',  ( 0.000000000000000000, -1.000000000000000000, 0.000000000000000000 ) ) ;
#14127 = CARTESIAN_POINT ( 'NONE',  ( 12.69999999999999929, -3599.497499999999945, 2263.571799999999712 ) ) ;
#14128 = CIRCLE ( 'NONE', #4018, 0.7619999999999294005 ) ;
#14129 = DIRECTION ( 'NONE',  ( -1.000000000000000000, 0.000000000000000000, 0.000000000000000000 ) ) ;
#14130 = VERTEX_POINT ( 'NONE', #13530 ) ;
#14131 = CALENDAR_DATE ( 2026, 26, 10 ) ;
#14132 = ORIENTED_EDGE ( 'NONE', *, *, #17845, .F. ) ;
#14133 = CARTESIAN_POINT ( 'NONE',  ( 139.6999999999999886, -3656.329999999999472, 2270.760000000000218 ) ) ;
#14134 = EDGE_CURVE ( 'NONE', #12899, #5417, #2359, .T. ) ;
#14135 = CARTESIAN_POINT ( 'NONE',  ( 10.77163876081882243, -3581.586621143886987, 2248.203750047890935 ) ) ;
#14136 = AXIS2_PLACEMENT_3D ( 'NONE', #20400, #6348, #4235 ) ;
#14137 = DIRECTION ( 'NONE',  ( 1.000000000000000000, 0.000000000000000000, 0.000000000000000000 ) ) ;
#14138 = ORIENTED_EDGE ( 'NONE', *, *, #16934, .F. ) ;
#14139 = LINE ( 'NONE', #16121, #22289 ) ;
#14140 = EDGE_CURVE ( 'NONE', #17496, #7479, #17039, .T. ) ;
#14141 = ADVANCED_FACE ( 'NONE', ( #11763 ), #17683, .T. ) ;
#14142 = EDGE_CURVE ( 'NONE', #287, #15612, #21445, .T. ) ;
#14143 = AXIS2_PLACEMENT_3D ( 'NONE', #10691, #21479, #3656 ) ;
#14144 = DIRECTION ( 'NONE',  ( -1.224646799147353207E-16, 1.000000000000000000, 0.000000000000000000 ) ) ;
#14145 = CARTESIAN_POINT ( 'NONE',  ( 6.985000000000000320, -3639.502500000000055, 2295.829799999999977 ) ) ;
#14146 = CARTESIAN_POINT ( 'NONE',  ( 11.34365660145000021, -3577.145744321000166, 2239.391000000000076 ) ) ;
#14147 = CARTESIAN_POINT ( 'NONE',  ( 12.17149329490156084, -3662.301214434115991, 2249.242076774587986 ) ) ;
#14148 = ORIENTED_EDGE ( 'NONE', *, *, #20279, .F. ) ;
#14149 =( REPRESENTATION_RELATIONSHIP ('NONE','NONE', #20448, #21348 ) REPRESENTATION_RELATIONSHIP_WITH_TRANSFORMATION ( #3321 )SHAPE_REPRESENTATION_RELATIONSHIP( ) );
#14150 = CARTESIAN_POINT ( 'NONE',  ( -8.890000000006001102, -3580.206200000000081, 2249.723686796999573 ) ) ;
#14151 = ORIENTED_EDGE ( 'NONE', *, *, #14461, .T. ) ;
#14152 = EDGE_CURVE ( 'NONE', #5186, #7425, #4585, .T. ) ;
#14153 = CARTESIAN_POINT ( 'NONE',  ( 142.5448000000000093, -3579.494999999999891, 2256.063560000000052 ) ) ;
#14154 = DIRECTION ( 'NONE',  ( -1.000000000000000000, 2.330758767201999921E-14, 2.343004830739999973E-14 ) ) ;
#14155 = VECTOR ( 'NONE', #436, 1000.000000000000000 ) ;
#14156 = DIRECTION ( 'NONE',  ( 0.000000000000000000, 0.000000000000000000, -1.000000000000000000 ) ) ;
#14157 = CARTESIAN_POINT ( 'NONE',  ( 14.97105788294492612, -3657.791708964490226, 2248.997938942161454 ) ) ;
#14158 = CARTESIAN_POINT ( 'NONE',  ( 137.0704399687386115, -3695.151712727613813, 2255.549808266575383 ) ) ;
#14159 = CARTESIAN_POINT ( 'NONE',  ( 9.993247422846968320, -3578.570632894392929, 2250.236801304443816 ) ) ;
#14160 = ADVANCED_FACE ( 'NONE', ( #20344 ), #9103, .T. ) ;
#14161 = ORIENTED_EDGE ( 'NONE', *, *, #21399, .F. ) ;
#14162 = DIRECTION ( 'NONE',  ( 1.000000000000000000, 0.000000000000000000, 0.000000000000000000 ) ) ;
#14163 = LINE ( 'NONE', #21652, #5926 ) ;
#14164 = COORDINATED_UNIVERSAL_TIME_OFFSET ( 0, 0, .AHEAD. ) ;
#14165 = DIRECTION ( 'NONE',  ( 0.000000000000000000, 1.000000000000000000, 0.000000000000000000 ) ) ;
#14166 = CARTESIAN_POINT ( 'NONE',  ( 20.32000000000000028, -3544.061999999999898, 2285.606299999999919 ) ) ;
#14167 = DIRECTION ( 'NONE',  ( 0.000000000000000000, -1.000000000000000000, 0.000000000000000000 ) ) ;
#14168 = ORIENTED_EDGE ( 'NONE', *, *, #7827, .T. ) ;
#14169 = CARTESIAN_POINT ( 'NONE',  ( 20.62424768829000143, -3544.570000000000164, 2260.600000000000364 ) ) ;
#14170 = ADVANCED_FACE ( 'NONE', ( #4286 ), #6984, .T. ) ;
#14171 = DIRECTION ( 'NONE',  ( 0.000000000000000000, 0.000000000000000000, -1.000000000000000000 ) ) ;
#14172 = AXIS2_PLACEMENT_3D ( 'NONE', #20773, #2613, #9757 ) ;
#14173 = ADVANCED_FACE ( 'NONE', ( #6746 ), #18442, .T. ) ;
#14174 = EDGE_CURVE ( 'NONE', #22625, #3671, #15647, .T. ) ;
#14175 = CARTESIAN_POINT ( 'NONE',  ( 38.10000000000000142, -3594.099999999999909, 2239.771999999999935 ) ) ;
#14176 = ORIENTED_EDGE ( 'NONE', *, *, #12681, .T. ) ;
#14177 = FACE_BOUND ( 'NONE', #4109, .T. ) ;
#14178 = DIRECTION ( 'NONE',  ( 2.336881798971000105E-14, 2.336881798971000105E-14, 1.000000000000000000 ) ) ;
#14179 = ORIENTED_EDGE ( 'NONE', *, *, #19921, .F. ) ;
#14180 = ADVANCED_FACE ( 'NONE', ( #12248 ), #6864, .F. ) ;
#14181 = DIRECTION ( 'NONE',  ( 0.000000000000000000, 1.000000000000000000, 0.000000000000000000 ) ) ;
#14182 = ORIENTED_EDGE ( 'NONE', *, *, #10651, .F. ) ;
#14183 = CARTESIAN_POINT ( 'NONE',  ( 142.7470794804999912, -3695.699999999999818, 2254.503999999999905 ) ) ;
#14184 = CARTESIAN_POINT ( 'NONE',  ( 127.0000000000000000, -3568.700000000000273, 2239.009999999999764 ) ) ;
#14185 = VERTEX_POINT ( 'NONE', #3096 ) ;
#14186 = ADVANCED_FACE ( 'NONE', ( #10479 ), #15877, .F. ) ;
#14187 = EDGE_LOOP ( 'NONE', ( #5995, #68, #6670, #18806 ) ) ;
#14188 = EDGE_CURVE ( 'NONE', #2684, #12318, #16923, .T. ) ;
#14189 = CARTESIAN_POINT ( 'NONE',  ( 139.6999999999999886, -3659.504999999999654, 2245.359999999999673 ) ) ;
#14190 = EDGE_LOOP ( 'NONE', ( #9654, #8196 ) ) ;
#14191 = DIRECTION ( 'NONE',  ( 0.000000000000000000, -1.000000000000000000, 0.000000000000000000 ) ) ;
#14192 = APPROVAL_ROLE ( '' ) ;
#14193 = CARTESIAN_POINT ( 'NONE',  ( 35.56000000000000227, -3568.700000000000273, 2247.392000000000280 ) ) ;
#14194 = CARTESIAN_POINT ( 'NONE',  ( 15.15106812040523998, -3580.939163279126660, 2249.333860731847835 ) ) ;
#14195 = CARTESIAN_POINT ( 'NONE',  ( 3.175000000091532382, -3544.061999999999898, 2275.001800000095045 ) ) ;
#14196 = DIRECTION ( 'NONE',  ( 1.224646799147353207E-16, 1.000000000000000000, -0.000000000000000000 ) ) ;
#14197 = CARTESIAN_POINT ( 'NONE',  ( 136.8552000000009912, -3659.504999999999654, 2272.030000000000200 ) ) ;
#14198 = VERTEX_POINT ( 'NONE', #23125 ) ;
#14199 = CARTESIAN_POINT ( 'NONE',  ( 15.48312395866995494, -3695.517456594313444, 2255.165366398894548 ) ) ;
#14200 = CARTESIAN_POINT ( 'NONE',  ( 20.32000000000000028, -3568.700000000000273, 2286.368300000000090 ) ) ;
#14201 = ORIENTED_EDGE ( 'NONE', *, *, #18115, .T. ) ;
#14202 = CARTESIAN_POINT ( 'NONE',  ( 4.806192532568648978, -3695.561367818985218, 2259.914321287728399 ) ) ;
#14203 = LINE ( 'NONE', #18055, #8752 ) ;
#14204 = CARTESIAN_POINT ( 'NONE',  ( 20.25432815364000305, -3544.321224993999749, 2260.506484774000000 ) ) ;
#14205 = ORIENTED_EDGE ( 'NONE', *, *, #5973, .F. ) ;
#14206 = PLANE ( 'NONE',  #8295 ) ;
#14207 = CARTESIAN_POINT ( 'NONE',  ( 9.987313202835000681, -3637.936329547143941, 2296.591799999999694 ) ) ;
#14208 = ORIENTED_EDGE ( 'NONE', *, *, #21769, .T. ) ;
#14209 = DIRECTION ( 'NONE',  ( -1.000000000000000000, 0.000000000000000000, 0.000000000000000000 ) ) ;
#14210 = DIRECTION ( 'NONE',  ( -0.6887494619146554697, 0.000000000000000000, -0.7249994335944496271 ) ) ;
#14211 = DIRECTION ( 'NONE',  ( 0.000000000000000000, 0.000000000000000000, -1.000000000000000000 ) ) ;
#14212 = SHAPE_DEFINITION_REPRESENTATION ( #16126, #8615 ) ;
#14213 = CIRCLE ( 'NONE', #3341, 2.844799999999994444 ) ;
#14214 = FACE_OUTER_BOUND ( 'NONE', #5269, .T. ) ;
#14215 = CARTESIAN_POINT ( 'NONE',  ( 9.787879217019574085, -3695.655085023491210, 2254.841286578994641 ) ) ;
#14216 = APPLIED_APPROVAL_ASSIGNMENT ( #16798, ( #20962 ) ) ;
#14217 = DIRECTION ( 'NONE',  ( 0.000000000000000000, 0.000000000000000000, -1.000000000000000000 ) ) ;
#14218 =( GEOMETRIC_REPRESENTATION_CONTEXT ( 3 ) GLOBAL_UNCERTAINTY_ASSIGNED_CONTEXT ( ( #7837 ) ) GLOBAL_UNIT_ASSIGNED_CONTEXT ( ( #5801, #6027, #14815 ) ) REPRESENTATION_CONTEXT ( 'NONE', 'WORKASPACE' ) );
#14219 = CARTESIAN_POINT ( 'NONE',  ( 137.0543742791004149, -3658.459229904648510, 2249.687221467814197 ) ) ;
#14220 = ORIENTED_EDGE ( 'NONE', *, *, #21889, .T. ) ;
#14221 = CARTESIAN_POINT ( 'NONE',  ( 3.175000000091532382, -3544.061999999999898, 2275.001800000095045 ) ) ;
#14222 = APPROVAL ( #3533, 'UNSPECIFIED' ) ;
#14223 = ORIENTED_EDGE ( 'NONE', *, *, #4521, .T. ) ;
#14224 = EDGE_LOOP ( 'NONE', ( #9171, #17346, #22265, #19399 ) ) ;
#14225 = ORIENTED_EDGE ( 'NONE', *, *, #17064, .F. ) ;
#14226 = CIRCLE ( 'NONE', #21337, 3.606799999999993567 ) ;
#14227 = CARTESIAN_POINT ( 'NONE',  ( 9.859719926546999247, -3579.298590683999919, 2250.205126089999794 ) ) ;
#14228 = EDGE_CURVE ( 'NONE', #6140, #3526, #5331, .T. ) ;
#14229 = ORIENTED_EDGE ( 'NONE', *, *, #1965, .F. ) ;
#14230 = ORIENTED_EDGE ( 'NONE', *, *, #706, .F. ) ;
#14231 = LOCAL_TIME ( 17, 37, 43.00000000000000000, #10578 ) ;
#14232 = DIRECTION ( 'NONE',  ( -2.334777064352623371E-14, -1.000000000000000000, 0.000000000000000000 ) ) ;
#14233 = EDGE_CURVE ( 'NONE', #19050, #11590, #7588, .T. ) ;
#14234 = APPROVAL_STATUS ( 'not_yet_approved' ) ;
#14235 = CARTESIAN_POINT ( 'NONE',  ( 0.000000000000000000, -3695.699999999999818, 2260.600000000000364 ) ) ;
#14236 = CARTESIAN_POINT ( 'NONE',  ( 12.69999999999999929, -3602.672500000000127, 2264.841800000000148 ) ) ;
#14237 = EDGE_CURVE ( 'NONE', #18263, #1122, #22912, .T. ) ;
#14238 = EDGE_LOOP ( 'NONE', ( #19753, #13710, #2653, #15860, #10906, #16039 ) ) ;
#14239 = CARTESIAN_POINT ( 'NONE',  ( 12.69999999999999929, -3653.789999999999964, 2262.355140000000119 ) ) ;
#14240 = FACE_BOUND ( 'NONE', #4878, .T. ) ;
#14241 = CARTESIAN_POINT ( 'NONE',  ( 25.39999999999999858, -3568.700000000000273, 2259.837999999999738 ) ) ;
#14242 = VERTEX_POINT ( 'NONE', #3216 ) ;
#14243 = CALENDAR_DATE ( 2026, 26, 10 ) ;
#14244 = ORIENTED_EDGE ( 'NONE', *, *, #20973, .T. ) ;
#14245 = EDGE_CURVE ( 'NONE', #20927, #15488, #18801, .T. ) ;
#14246 = CARTESIAN_POINT ( 'NONE',  ( 132.0221669333815555, -3543.967586182882769, 2260.455859883436005 ) ) ;
#14247 = AXIS2_PLACEMENT_3D ( 'NONE', #15916, #23048, #5373 ) ;
#14248 = DIRECTION ( 'NONE',  ( 0.000000000000000000, 1.000000000000000000, 0.000000000000000000 ) ) ;
#14249 = DIRECTION ( 'NONE',  ( 0.000000000000000000, 0.000000000000000000, 1.000000000000000000 ) ) ;
#14250 = CYLINDRICAL_SURFACE ( 'NONE', #8052, 1.269999999999993356 ) ;
#14251 = APPROVAL_PERSON_ORGANIZATION ( #3276, #15092, #10422 ) ;
#14252 = EDGE_LOOP ( 'NONE', ( #4916, #9369, #2153, #21331 ) ) ;
#14253 = LINE ( 'NONE', #5115, #11091 ) ;
#14254 = AXIS2_PLACEMENT_3D ( 'NONE', #5192, #13620, #20767 ) ;
#14255 = CARTESIAN_POINT ( 'NONE',  ( 9.987313202991520811, -3577.928829547366604, 2239.009999999999764 ) ) ;
#14256 = CARTESIAN_POINT ( 'NONE',  ( 117.1447999999989946, -3644.899999999999636, 2261.869999999999891 ) ) ;
#14257 = CYLINDRICAL_SURFACE ( 'NONE', #21232, 0.7619999999999294005 ) ;
#14258 = DIRECTION ( 'NONE',  ( 0.000000000000000000, -1.000000000000000000, 0.000000000000000000 ) ) ;
#14259 = CARTESIAN_POINT ( 'NONE',  ( 12.69997737250858982, -3642.347301253999831, 2279.817639304488239 ) ) ;
#14260 = EDGE_CURVE ( 'NONE', #6431, #12197, #17702, .T. ) ;
#14261 = ORIENTED_EDGE ( 'NONE', *, *, #4432, .F. ) ;
#14262 = DIRECTION ( 'NONE',  ( 1.000000000000000000, -2.334777064353000131E-14, -2.343004830739999973E-14 ) ) ;
#14263 = ADVANCED_FACE ( 'NONE', ( #8849 ), #7248, .T. ) ;
#14264 = DIRECTION ( 'NONE',  ( 0.000000000000000000, -1.000000000000000000, 0.000000000000000000 ) ) ;
#14265 = ADVANCED_FACE ( 'NONE', ( #12476 ), #2982, .T. ) ;
#14266 = CARTESIAN_POINT ( 'NONE',  ( -8.890000000026999416, -3576.167599999999766, 2247.392000000000280 ) ) ;
#14267 = CARTESIAN_POINT ( 'NONE',  ( 14.91356650787898275, -3657.717498031156993, 2248.884953215802398 ) ) ;
#14268 = CARTESIAN_POINT ( 'NONE',  ( 50.79999999999999716, -3619.500000000000000, 2261.869999999999891 ) ) ;
#14269 = APPLIED_APPROVAL_ASSIGNMENT ( #6767, ( #43 ) ) ;
#14270 = VERTEX_POINT ( 'NONE', #15523 ) ;
#14271 = LOCAL_TIME ( 17, 37, 43.00000000000000000, #7784 ) ;
#14272 = CARTESIAN_POINT ( 'NONE',  ( -6.349999999999999645, -3578.860000000000127, 2243.785200000000259 ) ) ;
#14273 = EDGE_LOOP ( 'NONE', ( #15717, #20803 ) ) ;
#14274 = DIRECTION ( 'NONE',  ( 0.000000000000000000, 0.000000000000000000, 1.000000000000000000 ) ) ;
#14275 = DIRECTION ( 'NONE',  ( 2.336881798971000105E-14, 2.336881798971000105E-14, 1.000000000000000000 ) ) ;
#14276 = DATE_AND_TIME ( #8885, #7156 ) ;
#14277 = AXIS2_PLACEMENT_3D ( 'NONE', #11889, #11532, #2627 ) ;
#14278 = DIRECTION ( 'NONE',  ( 0.000000000000000000, 0.000000000000000000, 1.000000000000000000 ) ) ;
#14279 = CARTESIAN_POINT ( 'NONE',  ( 12.69999999999999929, -3570.287499999999909, 2257.592639999999847 ) ) ;
#14280 = DIRECTION ( 'NONE',  ( 0.000000000000000000, 0.000000000000000000, 1.000000000000000000 ) ) ;
#14281 = FACE_OUTER_BOUND ( 'NONE', #18704, .T. ) ;
#14282 = ORIENTED_EDGE ( 'NONE', *, *, #14477, .T. ) ;
#14283 = DIRECTION ( 'NONE',  ( 0.000000000000000000, 2.331176954593720496E-12, -1.000000000000000000 ) ) ;
#14284 = ORIENTED_EDGE ( 'NONE', *, *, #17226, .T. ) ;
#14285 = CARTESIAN_POINT ( 'NONE',  ( 12.69999999999999929, -3639.502500000000055, 2288.971800000000258 ) ) ;
#14286 = FACE_OUTER_BOUND ( 'NONE', #4984, .T. ) ;
#14287 = EDGE_LOOP ( 'NONE', ( #2548, #14630, #1565, #19508 ) ) ;
#14288 = CARTESIAN_POINT ( 'NONE',  ( 35.56000000000031491, -3568.700000000000273, 2250.236800000000130 ) ) ;
#14289 = AXIS2_PLACEMENT_3D ( 'NONE', #22896, #6753, #15655 ) ;
#14290 = CIRCLE ( 'NONE', #7181, 2.844800000000091700 ) ;
#14291 = ORIENTED_EDGE ( 'NONE', *, *, #2776, .F. ) ;
#14292 = CARTESIAN_POINT ( 'NONE',  ( 142.4828652621451681, -3695.514947976519579, 2255.165528820269174 ) ) ;
#14293 = DIRECTION ( 'NONE',  ( 0.000000000000000000, 1.000000000000000000, 0.000000000000000000 ) ) ;
#14294 = VERTEX_POINT ( 'NONE', #12007 ) ;
#14295 = VERTEX_POINT ( 'NONE', #22662 ) ;
#14296 = ADVANCED_FACE ( 'NONE', ( #10245 ), #6636, .T. ) ;
#14297 = EDGE_CURVE ( 'NONE', #14270, #7196, #1569, .T. ) ;
#14298 = CARTESIAN_POINT ( 'NONE',  ( 136.9934899154386301, -3580.373043272544237, 2249.801989270562899 ) ) ;
#14299 = ORIENTED_EDGE ( 'NONE', *, *, #22587, .F. ) ;
#14300 = DIRECTION ( 'NONE',  ( 0.000000000000000000, 0.000000000000000000, 1.000000000000000000 ) ) ;
#14301 =( BOUNDED_CURVE ( )  B_SPLINE_CURVE ( 3, ( #1535, #17584, #20760, #13614 ),
 .UNSPECIFIED., .F., .T. ) 
 B_SPLINE_CURVE_WITH_KNOTS ( ( 4, 4 ),
 ( 3.673835071120097305E-14, 1.570796326490076611 ),
 .UNSPECIFIED. ) 
 CURVE ( )  GEOMETRIC_REPRESENTATION_ITEM ( )  RATIONAL_B_SPLINE_CURVE ( ( 1.000000000000000000, 0.8047378541962203480, 0.8047378541962203480, 1.000000000000000000 ) ) 
 REPRESENTATION_ITEM ( '' )  );
#14302 = PERSON_AND_ORGANIZATION ( #5446, #1895 ) ;
#14303 = CARTESIAN_POINT ( 'NONE',  ( 116.8400000000003160, -3568.700000000000273, 2250.236800000000130 ) ) ;
#14304 = LINE ( 'NONE', #5633, #8879 ) ;
#14305 = EDGE_CURVE ( 'NONE', #15808, #15441, #15084, .T. ) ;
#14306 = AXIS2_PLACEMENT_3D ( 'NONE', #8590, #964, #6726 ) ;
#14307 = FACE_OUTER_BOUND ( 'NONE', #10481, .T. ) ;
#14308 = CARTESIAN_POINT ( 'NONE',  ( 12.69999999999999929, -3599.497499999999945, 2296.210799999999836 ) ) ;
#14309 = CIRCLE ( 'NONE', #12794, 1.269999999999882334 ) ;
#14310 = CARTESIAN_POINT ( 'NONE',  ( 76.20000000000000284, -3670.300000000000182, 2239.009999999999764 ) ) ;
#14311 = EDGE_LOOP ( 'NONE', ( #1975, #9453, #9640, #14710 ) ) ;
#14312 = CARTESIAN_POINT ( 'NONE',  ( 134.5774142888278391, -3576.960814571373248, 2245.272442446700552 ) ) ;
#14313 = EDGE_CURVE ( 'NONE', #10134, #5650, #7205, .T. ) ;
#14314 = EDGE_CURVE ( 'NONE', #10278, #1882, #16583, .T. ) ;
#14315 = FACE_OUTER_BOUND ( 'NONE', #15188, .T. ) ;
#14316 = EDGE_LOOP ( 'NONE', ( #14617, #16051, #19567, #13327 ) ) ;
#14317 = CARTESIAN_POINT ( 'NONE',  ( -12.31900000000000084, -3662.489255679000053, 2248.748343399000532 ) ) ;
#14318 = FACE_OUTER_BOUND ( 'NONE', #9297, .T. ) ;
#14319 = AXIS2_PLACEMENT_3D ( 'NONE', #19169, #8510, #6872 ) ;
#14320 = CYLINDRICAL_SURFACE ( 'NONE', #3933, 0.7619999999999294005 ) ;
#14321 = ORIENTED_EDGE ( 'NONE', *, *, #7805, .F. ) ;
#14322 = LINE ( 'NONE', #14440, #7946 ) ;
#14323 = TOROIDAL_SURFACE ( 'NONE', #16189, 6.477000000000000313, 0.7620000000000000107 ) ;
#14324 = FACE_OUTER_BOUND ( 'NONE', #2949, .T. ) ;
#14325 = CIRCLE ( 'NONE', #22898, 5.714999999999995417 ) ;
#14326 = ORIENTED_EDGE ( 'NONE', *, *, #20668, .T. ) ;
#14327 = VECTOR ( 'NONE', #4773, 1000.000000000000000 ) ;
#14328 = CARTESIAN_POINT ( 'NONE',  ( -6.349999999999999645, -3575.684999999999945, 2247.392000000000280 ) ) ;
#14329 = EDGE_CURVE ( 'NONE', #3812, #18833, #22562, .T. ) ;
#14330 = DIRECTION ( 'NONE',  ( 1.000000000000000000, 0.000000000000000000, 0.000000000000000000 ) ) ;
#14331 = SHAPE_REPRESENTATION_RELATIONSHIP ( 'NONE' , 'NONE' ,  #13400, #9094 ) ;
#14332 = DIRECTION ( 'NONE',  ( -0.000000000000000000, -1.000000000000000000, -0.000000000000000000 ) ) ;
#14333 = FACE_BOUND ( 'NONE', #1098, .T. ) ;
#14334 = PERSON_AND_ORGANIZATION_ROLE ( 'creator' ) ;
#14335 = DIRECTION ( 'NONE',  ( 0.000000000000000000, 0.000000000000000000, 1.000000000000000000 ) ) ;
#14336 = DIRECTION ( 'NONE',  ( 0.000000000000000000, 0.000000000000000000, 1.000000000000000000 ) ) ;
#14337 = ORIENTED_EDGE ( 'NONE', *, *, #15846, .T. ) ;
#14338 = CARTESIAN_POINT ( 'NONE',  ( 139.6999999999999886, -3659.504999999999654, 2272.030000000000200 ) ) ;
#14339 = AXIS2_PLACEMENT_3D ( 'NONE', #1554, #15859, #4606 ) ;
#14340 = CARTESIAN_POINT ( 'NONE',  ( 137.0509968171786568, -3658.467794019345547, 2249.693473747279768 ) ) ;
#14341 = VERTEX_POINT ( 'NONE', #2277 ) ;
#14342 = AXIS2_PLACEMENT_3D ( 'NONE', #4746, #9559, #16704 ) ;
#14343 = CARTESIAN_POINT ( 'NONE',  ( 98.75520000000000209, -3670.300000000000182, 2239.771999999999935 ) ) ;
#14344 = AXIS2_PLACEMENT_3D ( 'NONE', #13185, #2530, #16705 ) ;
#14345 = ORIENTED_EDGE ( 'NONE', *, *, #220, .F. ) ;
#14346 = ORIENTED_EDGE ( 'NONE', *, *, #16727, .T. ) ;
#14347 = EDGE_LOOP ( 'NONE', ( #6417, #6972 ) ) ;
#14348 = CYLINDRICAL_SURFACE ( 'NONE', #609, 2.844800000000091700 ) ;
#14349 = ORIENTED_EDGE ( 'NONE', *, *, #7240, .F. ) ;
#14350 = ORIENTED_EDGE ( 'NONE', *, *, #6576, .F. ) ;
#14351 = CARTESIAN_POINT ( 'NONE',  ( 123.3932000000010021, -3568.700000000000273, 2239.771999999999935 ) ) ;
#14352 = LINE ( 'NONE', #19971, #909 ) ;
#14353 = AXIS2_PLACEMENT_3D ( 'NONE', #11134, #9486, #18619 ) ;
#14354 = CARTESIAN_POINT ( 'NONE',  ( 147.3199999999999932, -3694.430000000000291, 2260.600000000000364 ) ) ;
#14355 = ORIENTED_EDGE ( 'NONE', *, *, #14891, .F. ) ;
#14356 = CARTESIAN_POINT ( 'NONE',  ( -5.588000000000000078, -3695.699999999999818, 2229.612000000000080 ) ) ;
#14357 = CARTESIAN_POINT ( 'NONE',  ( 152.4000000000000057, -3695.699999999999818, 2275.001800000000003 ) ) ;
#14358 = CARTESIAN_POINT ( 'NONE',  ( 6.985000002048999512, -3579.494756921999851, 2244.617465693000213 ) ) ;
#14359 = FACE_OUTER_BOUND ( 'NONE', #15768, .T. ) ;
#14360 = APPROVAL_ROLE ( '' ) ;
#14361 = APPLIED_DATE_AND_TIME_ASSIGNMENT ( #3556, #21378, ( #15394 ) ) ;
#14362 = ORIENTED_EDGE ( 'NONE', *, *, #15310, .T. ) ;
#14363 = CARTESIAN_POINT ( 'NONE',  ( 131.7443772039423493, -3543.374810890516983, 2259.759470120345213 ) ) ;
#14364 = ORIENTED_EDGE ( 'NONE', *, *, #6540, .F. ) ;
#14365 = LINE ( 'NONE', #19865, #6823 ) ;
#14366 = EDGE_CURVE ( 'NONE', #5595, #3108, #14701, .T. ) ;
#14367 = DIRECTION ( 'NONE',  ( 0.000000000000000000, 0.000000000000000000, -1.000000000000000000 ) ) ;
#14368 = ORIENTED_EDGE ( 'NONE', *, *, #6925, .F. ) ;
#14369 = AXIS2_PLACEMENT_3D ( 'NONE', #10319, #5285, #15947 ) ;
#14370 = DIRECTION ( 'NONE',  ( 0.000000000000000000, -1.000000000000000000, 0.000000000000000000 ) ) ;
#14371 = DIRECTION ( 'NONE',  ( 0.000000000000000000, 0.000000000000000000, -1.000000000000000000 ) ) ;
#14372 = CARTESIAN_POINT ( 'NONE',  ( 9.956800000000452400, -3580.373257047480820, 2255.967039999999997 ) ) ;
#14373 = DIRECTION ( 'NONE',  ( 0.000000000000000000, 0.000000000000000000, -1.000000000000000000 ) ) ;
#14374 = DIRECTION ( 'NONE',  ( 0.000000000000000000, 0.000000000000000000, 1.000000000000000000 ) ) ;
#14375 = CARTESIAN_POINT ( 'NONE',  ( 12.69999999999999929, -3579.494999999999891, 2272.030000000000200 ) ) ;
#14376 = VERTEX_POINT ( 'NONE', #14476 ) ;
#14377 = DIRECTION ( 'NONE',  ( 0.000000000000000000, 0.000000000000000000, 1.000000000000000000 ) ) ;
#14378 = DIRECTION ( 'NONE',  ( -1.000000000000000000, 0.000000000000000000, -8.741913579724999851E-14 ) ) ;
#14379 = LINE ( 'NONE', #20119, #18189 ) ;
#14380 = DIRECTION ( 'NONE',  ( 0.000000000000000000, 0.000000000000000000, 1.000000000000000000 ) ) ;
#14381 = CARTESIAN_POINT ( 'NONE',  ( 142.3546999974072378, -3543.765301130966236, 2255.486749947766384 ) ) ;
#14382 = CARTESIAN_POINT ( 'NONE',  ( 136.8622528204724063, -3695.586719555755280, 2255.028339697612864 ) ) ;
#14383 = ORIENTED_EDGE ( 'NONE', *, *, #14723, .T. ) ;
#14384 = CIRCLE ( 'NONE', #22589, 2.844800000000001550 ) ;
#14385 = CARTESIAN_POINT ( 'NONE',  ( 7.181610858756661386, -3578.008765548840984, 2244.677489325244096 ) ) ;
#14386 = ORIENTED_EDGE ( 'NONE', *, *, #14544, .T. ) ;
#14387 = APPROVAL ( #9082, 'UNSPECIFIED' ) ;
#14388 = CIRCLE ( 'NONE', #13249, 5.460999999999938126 ) ;
#14389 = CARTESIAN_POINT ( 'NONE',  ( 64.76999999999999602, -3670.300000000000182, 2289.213099999999940 ) ) ;
#14390 = DATE_TIME_ROLE ( 'classification_date' ) ;
#14391 = DIRECTION ( 'NONE',  ( -1.000000000000000000, 0.000000000000000000, 0.000000000000000000 ) ) ;
#14392 = EDGE_CURVE ( 'NONE', #22551, #20085, #21951, .T. ) ;
#14393 = CARTESIAN_POINT ( 'NONE',  ( 9.864068217991999177, -3659.229970544000025, 2257.960591680000107 ) ) ;
#14394 = DIRECTION ( 'NONE',  ( 1.122008997397786234E-13, 0.000000000000000000, 1.000000000000000000 ) ) ;
#14395 = EDGE_CURVE ( 'NONE', #15888, #16359, #19858, .T. ) ;
#14396 = CYLINDRICAL_SURFACE ( 'NONE', #21250, 2.844799999999994444 ) ;
#14397 = EDGE_CURVE ( 'NONE', #957, #17884, #7322, .T. ) ;
#14398 = VERTEX_POINT ( 'NONE', #18094 ) ;
#14399 = CIRCLE ( 'NONE', #15886, 11.11250000000000071 ) ;
#14400 = DIRECTION ( 'NONE',  ( 0.000000000000000000, -0.8660254037817070039, 0.5000000000047313264 ) ) ;
#14401 = AXIS2_PLACEMENT_3D ( 'NONE', #5821, #8867, #7111 ) ;
#14402 = DIRECTION ( 'NONE',  ( -0.6887494619146554697, 0.000000000000000000, -0.7249994335944496271 ) ) ;
#14403 = AXIS2_PLACEMENT_3D ( 'NONE', #5097, #12240, #1685 ) ;
#14404 = ORIENTED_EDGE ( 'NONE', *, *, #1797, .T. ) ;
#14405 = FACE_OUTER_BOUND ( 'NONE', #4444, .T. ) ;
#14406 = ORIENTED_EDGE ( 'NONE', *, *, #12141, .F. ) ;
#14407 = CARTESIAN_POINT ( 'NONE',  ( 142.5173730182035285, -3695.562642950982081, 2255.079208150718387 ) ) ;
#14408 = DIRECTION ( 'NONE',  ( 0.000000000000000000, 0.000000000000000000, -1.000000000000000000 ) ) ;
#14409 = EDGE_CURVE ( 'NONE', #4689, #10096, #4035, .T. ) ;
#14410 = PERSON ( 'NAUO-PER15', 'UNSPECIFIED', 'UNSPECIFIED', ('UNSPECIFIED'), ('UNSPECIFIED'), ('UNSPECIFIED') ) ;
#14411 = ORIENTED_EDGE ( 'NONE', *, *, #13824, .F. ) ;
#14412 = CARTESIAN_POINT ( 'NONE',  ( 137.9083009636803467, -3581.704713601686308, 2247.346194313388423 ) ) ;
#14413 = CIRCLE ( 'NONE', #10713, 5.460999999999938126 ) ;
#14414 = ORIENTED_EDGE ( 'NONE', *, *, #15229, .F. ) ;
#14415 = CARTESIAN_POINT ( 'NONE',  ( 139.6999999999999886, -3582.339799999999286, 2257.592639999999847 ) ) ;
#14416 = AXIS2_PLACEMENT_3D ( 'NONE', #14941, #644, #7793 ) ;
#14417 = PERSON_AND_ORGANIZATION_ROLE ( 'creator' ) ;
#14418 = AXIS2_PLACEMENT_3D ( 'NONE', #19010, #18889, #2833 ) ;
#14419 = DIRECTION ( 'NONE',  ( 0.8928571428573600643, -0.4503400076038009403, 0.000000000000000000 ) ) ;
#14420 = DIRECTION ( 'NONE',  ( 0.000000000000000000, 0.000000000000000000, 1.000000000000000000 ) ) ;
#14421 = CARTESIAN_POINT ( 'NONE',  ( 15.03168679716618605, -3578.148799999850326, 2239.167815367177809 ) ) ;
#14422 = EDGE_CURVE ( 'NONE', #12415, #10003, #13314, .T. ) ;
#14423 = DIRECTION ( 'NONE',  ( -0.8660254037825932949, 0.5000000000031962211, 0.000000000000000000 ) ) ;
#14424 = CARTESIAN_POINT ( 'NONE',  ( 142.1563837964497168, -3578.059926228095264, 2250.122030119480769 ) ) ;
#14425 = ORIENTED_EDGE ( 'NONE', *, *, #15609, .T. ) ;
#14426 = CARTESIAN_POINT ( 'NONE',  ( 134.7476930285313870, -3576.642325314609479, 2245.609748385880266 ) ) ;
#14427 = ADVANCED_FACE ( 'NONE', ( #19624 ), #20691, .T. ) ;
#14428 = EDGE_CURVE ( 'NONE', #19336, #1398, #10719, .T. ) ;
#14429 = CARTESIAN_POINT ( 'NONE',  ( 14.71514678359000072, -3577.480332084000111, 2257.776246897999954 ) ) ;
#14430 = EDGE_LOOP ( 'NONE', ( #14866, #9058, #1460, #7162, #18409, #21136, #9469, #18953, #809, #12037 ) ) ;
#14431 = B_SPLINE_CURVE_WITH_KNOTS ( 'NONE', 3,
 ( #18512, #704, #13232, #11584, #11476, #4220, #804, #11143, #16523, #5990, #7617, #475, #9388, #4337, #18732, #22363, #11253, #9829, #16759, #18397, #6219, #14776, #9612, #21917 ),
 .UNSPECIFIED., .F., .F.,
 ( 4, 2, 2, 1, 1, 1, 2, 2, 2, 2, 1, 2, 2, 4 ),
 ( 0.000000000000000000, 0.1249999999974724663, 0.1874999999964171993, 0.2187499999956769026, 0.2343749999957942254, 0.2421874999958534558, 0.2460937499958825159, 0.2499999999959115482, 0.3749999999939945816, 0.4374999999928649852, 0.4687499999920584082, 0.4843749999916692750, 0.4999999999912801973, 1.000000000000000000 ),
 .UNSPECIFIED. ) ;
#14432 = AXIS2_PLACEMENT_3D ( 'NONE', #20634, #9638, #16665 ) ;
#14433 = CARTESIAN_POINT ( 'NONE',  ( 4.762728537569663523, -3695.607672419785104, 2259.805487872981303 ) ) ;
#14434 = B_SPLINE_CURVE_WITH_KNOTS ( 'NONE', 3,
 ( #9933, #8306, #8189, #17431 ),
 .UNSPECIFIED., .F., .F.,
 ( 4, 4 ),
 ( 0.000000000000000000, 1.000000000000000000 ),
 .UNSPECIFIED. ) ;
#14435 = CARTESIAN_POINT ( 'NONE',  ( 73.35520000000001062, -3568.700000000000273, 2261.869999999999891 ) ) ;
#14436 = AXIS2_PLACEMENT_3D ( 'NONE', #18729, #19088, #17320 ) ;
#14437 = AXIS2_PLACEMENT_3D ( 'NONE', #7943, #2769, #678 ) ;
#14438 = CIRCLE ( 'NONE', #4309, 2.844800000000091700 ) ;
#14439 = ORIENTED_EDGE ( 'NONE', *, *, #16999, .T. ) ;
#14440 = CARTESIAN_POINT ( 'NONE',  ( 137.1599999999999966, -3694.430000000000291, 2255.774000000000342 ) ) ;
#14441 = PLANE ( 'NONE',  #2811 ) ;
#14442 = AXIS2_PLACEMENT_3D ( 'NONE', #17578, #3167, #20875 ) ;
#14443 = ORIENTED_EDGE ( 'NONE', *, *, #18377, .F. ) ;
#14444 = CARTESIAN_POINT ( 'NONE',  ( 12.69999999999999929, -3570.287499999999909, 2268.705139999999574 ) ) ;
#14445 = FACE_OUTER_BOUND ( 'NONE', #15058, .T. ) ;
#14446 = DIRECTION ( 'NONE',  ( 0.000000000000000000, 1.000000000000000000, 1.224646799147353207E-16 ) ) ;
#14447 = DIRECTION ( 'NONE',  ( -1.000000000000000000, 0.000000000000000000, 0.000000000000000000 ) ) ;
#14448 = ADVANCED_FACE ( 'NONE', ( #9079 ), #173, .T. ) ;
#14449 = COORDINATED_UNIVERSAL_TIME_OFFSET ( 0, 0, .AHEAD. ) ;
#14450 = CARTESIAN_POINT ( 'NONE',  ( 12.69999999999999929, -3655.060000000000400, 2268.705139999999574 ) ) ;
#14451 = CARTESIAN_POINT ( 'NONE',  ( 10.16000000000000014, -3694.430000000000291, 2255.774000000000342 ) ) ;
#14452 = EDGE_LOOP ( 'NONE', ( #10020, #8661, #22223 ) ) ;
#14453 = CARTESIAN_POINT ( 'NONE',  ( 18.22054351403157924, -3580.973142365039621, 2245.487016238938850 ) ) ;
#14454 = CIRCLE ( 'NONE', #4335, 2.844799999999994444 ) ;
#14455 = CIRCLE ( 'NONE', #3209, 1.524000000000000021 ) ;
#14456 = CARTESIAN_POINT ( 'NONE',  ( 137.5955831568913936, -3657.590698734706621, 2248.654663951603197 ) ) ;
#14457 = AXIS2_PLACEMENT_3D ( 'NONE', #13647, #8847, #3094 ) ;
#14458 = ORIENTED_EDGE ( 'NONE', *, *, #10084, .T. ) ;
#14459 = VECTOR ( 'NONE', #3110, 1000.000000000000000 ) ;
#14460 = CARTESIAN_POINT ( 'NONE',  ( 139.9704182635913128, -3662.340201044270998, 2249.195591307148334 ) ) ;
#14461 = EDGE_CURVE ( 'NONE', #12349, #21351, #500, .T. ) ;
#14462 = VERTEX_POINT ( 'NONE', #18771 ) ;
#14463 = EDGE_LOOP ( 'NONE', ( #17237, #3246 ) ) ;
#14464 = CARTESIAN_POINT ( 'NONE',  ( 9.855190710340998805, -3579.495000415000050, 2250.165025612000136 ) ) ;
#14465 = ORIENTED_EDGE ( 'NONE', *, *, #16446, .T. ) ;
#14466 = ORIENTED_EDGE ( 'NONE', *, *, #19982, .T. ) ;
#14467 = CARTESIAN_POINT ( 'NONE',  ( 12.69999999994000106, -3636.810100000000148, 2292.781800000000203 ) ) ;
#14468 = CIRCLE ( 'NONE', #11077, 2.844799999999994444 ) ;
#14469 = CONTEXT_DEPENDENT_SHAPE_REPRESENTATION ( #20877, #13520 ) ;
#14470 = CARTESIAN_POINT ( 'NONE',  ( 10.16000000000000014, -3694.430000000000291, 2255.774000000000342 ) ) ;
#14471 = CARTESIAN_POINT ( 'NONE',  ( 127.0000000000000000, -3568.700000000000273, 2259.837999999999738 ) ) ;
#14472 = ORIENTED_EDGE ( 'NONE', *, *, #2941, .T. ) ;
#14473 = CIRCLE ( 'NONE', #18955, 0.3809999999999993947 ) ;
#14474 = DIRECTION ( 'NONE',  ( 1.000000000000000000, 0.000000000000000000, 0.000000000000000000 ) ) ;
#14475 = CARTESIAN_POINT ( 'NONE',  ( 10.16000000000000014, -3578.213872745999652, 2255.774000000000342 ) ) ;
#14476 = CARTESIAN_POINT ( 'NONE',  ( 132.0583097651000060, -3544.202533098000458, 2260.545675974999995 ) ) ;
#14477 = EDGE_CURVE ( 'NONE', #10014, #20881, #6492, .T. ) ;
#14478 = DIRECTION ( 'NONE',  ( 0.000000000000000000, -1.000000000000000000, 4.457650181899999573E-12 ) ) ;
#14479 = VECTOR ( 'NONE', #16092, 1000.000000000000000 ) ;
#14480 = ADVANCED_FACE ( 'NONE', ( #6028 ), #13160, .F. ) ;
#14481 = DATE_AND_TIME ( #8853, #44 ) ;
#14482 = ORIENTED_EDGE ( 'NONE', *, *, #15685, .F. ) ;
#14483 = AXIS2_PLACEMENT_3D ( 'NONE', #10148, #673, #6071 ) ;
#14484 = CARTESIAN_POINT ( 'NONE',  ( 57.14999999999999858, -3694.430000000000291, 2250.236800000000130 ) ) ;
#14485 = ORIENTED_EDGE ( 'NONE', *, *, #22461, .T. ) ;
#14486 = CARTESIAN_POINT ( 'NONE',  ( 16.19063073443439293, -3695.699999999999818, 2282.113800000095125 ) ) ;
#14487 = DIRECTION ( 'NONE',  ( 0.000000000000000000, 0.000000000000000000, -1.000000000000000000 ) ) ;
#14488 = ORIENTED_EDGE ( 'NONE', *, *, #10015, .T. ) ;
#14489 = DIRECTION ( 'NONE',  ( 0.000000000000000000, 0.000000000000000000, -1.000000000000000000 ) ) ;
#14490 = AXIS2_PLACEMENT_3D ( 'NONE', #10947, #9197, #4482 ) ;
#14491 = DIRECTION ( 'NONE',  ( 0.000000000000000000, 1.000000000000000000, 0.000000000000000000 ) ) ;
#14492 = AXIS2_PLACEMENT_3D ( 'NONE', #7249, #8770, #21425 ) ;
#14493 = DIRECTION ( 'NONE',  ( 0.000000000000000000, 0.000000000000000000, -1.000000000000000000 ) ) ;
#14494 = AXIS2_PLACEMENT_3D ( 'NONE', #19262, #8715, #15861 ) ;
#14495 = CARTESIAN_POINT ( 'NONE',  ( 15.87499999973130826, -3695.384369265537771, 2281.351799999999912 ) ) ;
#14496 = CARTESIAN_POINT ( 'NONE',  ( 18.02447335878156665, -3657.428416424212173, 2246.524741530415668 ) ) ;
#14497 = ORIENTED_EDGE ( 'NONE', *, *, #1065, .T. ) ;
#14498 = DIRECTION ( 'NONE',  ( -1.000000000000000000, 0.000000000000000000, 0.000000000000000000 ) ) ;
#14499 = FACE_OUTER_BOUND ( 'NONE', #16228, .T. ) ;
#14500 = DIRECTION ( 'NONE',  ( 0.000000000000000000, 0.000000000000000000, -1.000000000000000000 ) ) ;
#14501 = CARTESIAN_POINT ( 'NONE',  ( 139.6999999999999886, -3668.712499999999636, 2279.817639999999756 ) ) ;
#14502 = CARTESIAN_POINT ( 'NONE',  ( 124.1552000000010025, -3568.700000000000273, 2239.771999999999935 ) ) ;
#14503 = CARTESIAN_POINT ( 'NONE',  ( 137.0197862866483831, -3695.306816721486484, 2255.422793245717912 ) ) ;
#14504 = ORIENTED_EDGE ( 'NONE', *, *, #19140, .T. ) ;
#14505 = CARTESIAN_POINT ( 'NONE',  ( 7.635186067085399486, -3576.847633590237820, 2245.381158637630051 ) ) ;
#14506 = ORIENTED_EDGE ( 'NONE', *, *, #14814, .F. ) ;
#14507 = APPROVAL_DATE_TIME ( #11100, #17811 ) ;
#14508 = AXIS2_PLACEMENT_3D ( 'NONE', #7629, #22259, #2697 ) ;
#14509 = DIRECTION ( 'NONE',  ( 1.000000000000000000, 0.000000000000000000, 0.000000000000000000 ) ) ;
#14510 = CARTESIAN_POINT ( 'NONE',  ( 25.39999999999999858, -3619.500000000000000, 2239.771999999999935 ) ) ;
#14511 = DATE_TIME_ROLE ( 'classification_date' ) ;
#14512 = CIRCLE ( 'NONE', #1018, 3.606799999998994366 ) ;
#14513 = FACE_OUTER_BOUND ( 'NONE', #1424, .T. ) ;
#14514 = CARTESIAN_POINT ( 'NONE',  ( 131.5729205195000020, -3543.299999999999727, 2259.329999999999927 ) ) ;
#14515 = DIRECTION ( 'NONE',  ( -1.000000000000000000, 0.000000000000000000, 0.000000000000000000 ) ) ;
#14516 = AXIS2_PLACEMENT_3D ( 'NONE', #18742, #2808, #1049 ) ;
#14517 = DIRECTION ( 'NONE',  ( 1.000000000000000000, 0.000000000000000000, 0.000000000000000000 ) ) ;
#14518 = DIRECTION ( 'NONE',  ( 0.000000000000000000, 0.000000000000000000, -1.000000000000000000 ) ) ;
#14519 = ORIENTED_EDGE ( 'NONE', *, *, #9247, .F. ) ;
#14520 = PLANE ( 'NONE',  #18920 ) ;
#14521 = APPLIED_PERSON_AND_ORGANIZATION_ASSIGNMENT ( #2172, #4148, ( #12786 ) ) ;
#14522 = VECTOR ( 'NONE', #5493, 1000.000000000000000 ) ;
#14523 = FACE_OUTER_BOUND ( 'NONE', #9443, .T. ) ;
#14524 = ORIENTED_EDGE ( 'NONE', *, *, #19599, .F. ) ;
#14525 = DIRECTION ( 'NONE',  ( 0.000000000000000000, 0.000000000000000000, 1.000000000000000000 ) ) ;
#14526 = AXIS2_PLACEMENT_3D ( 'NONE', #4382, #16906, #18669 ) ;
#14527 = ADVANCED_FACE ( 'NONE', ( #13270 ), #22173, .T. ) ;
#14528 = ORIENTED_EDGE ( 'NONE', *, *, #16323, .F. ) ;
#14529 = CARTESIAN_POINT ( 'NONE',  ( 142.5056715281748154, -3695.547111919549934, 2255.108476226979292 ) ) ;
#14530 = DIRECTION ( 'NONE',  ( -3.130242492740591634E-14, 0.000000000000000000, -1.000000000000000000 ) ) ;
#14531 = ADVANCED_FACE ( 'NONE', ( #16899 ), #6370, .T. ) ;
#14532 = ORIENTED_EDGE ( 'NONE', *, *, #12562, .T. ) ;
#14533 = EDGE_CURVE ( 'NONE', #18508, #21577, #7977, .T. ) ;
#14534 = CARTESIAN_POINT ( 'NONE',  ( 137.5722701175336908, -3581.383294861765989, 2248.705728950628327 ) ) ;
#14535 = ORIENTED_EDGE ( 'NONE', *, *, #11069, .F. ) ;
#14536 = CARTESIAN_POINT ( 'NONE',  ( 47.19319999999999737, -3619.500000000000000, 2239.771999999999935 ) ) ;
#14537 = APPLICATION_PROTOCOL_DEFINITION ( 'international standard', 'automotive_design', 2000, #4108 ) ;
#14538 = VECTOR ( 'NONE', #18188, 1000.000000000000000 ) ;
#14539 = DIRECTION ( 'NONE',  ( 1.000000000000000000, 0.000000000000000000, 0.000000000000000000 ) ) ;
#14540 = EDGE_CURVE ( 'NONE', #19756, #6235, #4246, .T. ) ;
#14541 = DIRECTION ( 'NONE',  ( 5.154430176750962410E-12, -0.5000000000031962211, 0.8660254037825932949 ) ) ;
#14542 = CARTESIAN_POINT ( 'NONE',  ( -12.31900000000000084, -3658.793800000000374, 2245.060313203000078 ) ) ;
#14543 = DIRECTION ( 'NONE',  ( 0.000000000000000000, 0.000000000000000000, -1.000000000000000000 ) ) ;
#14544 = EDGE_CURVE ( 'NONE', #9562, #22886, #138, .T. ) ;
#14545 = CARTESIAN_POINT ( 'NONE',  ( 141.0188720128104762, -3576.974003297035779, 2249.521926086513304 ) ) ;
#14546 = EDGE_LOOP ( 'NONE', ( #2801, #10924, #21020, #11145 ) ) ;
#14547 = CARTESIAN_POINT ( 'NONE',  ( 134.4979089453188692, -3577.128741457883280, 2245.134603798921034 ) ) ;
#14548 = EDGE_LOOP ( 'NONE', ( #10386, #12903, #4184, #9975, #17912 ) ) ;
#14549 = DIRECTION ( 'NONE',  ( 1.000000000000000000, 0.000000000000000000, 0.000000000000000000 ) ) ;
#14550 = EDGE_LOOP ( 'NONE', ( #17938, #4199, #1153, #12294 ) ) ;
#14551 = CARTESIAN_POINT ( 'NONE',  ( 10.18227454630999951, -3580.829269783999734, 2257.881334183000035 ) ) ;
#14552 = CARTESIAN_POINT ( 'NONE',  ( 64.76999999999999602, -3670.300000000000182, 2289.213099999999940 ) ) ;
#14553 = EDGE_LOOP ( 'NONE', ( #20860, #4365, #14942 ) ) ;
#14554 = LINE ( 'NONE', #16070, #21026 ) ;
#14555 = CARTESIAN_POINT ( 'NONE',  ( 95.25000000000000000, -3695.699999999999818, 2251.506800000000112 ) ) ;
#14556 = AXIS2_PLACEMENT_3D ( 'NONE', #7260, #16046, #10649 ) ;
#14557 = EDGE_CURVE ( 'NONE', #8066, #2758, #9479, .T. ) ;
#14558 = VERTEX_POINT ( 'NONE', #630 ) ;
#14559 = ADVANCED_FACE ( 'NONE', ( #2607 ), #18547, .T. ) ;
#14560 = CARTESIAN_POINT ( 'NONE',  ( 12.70000000003999929, -3582.187399999999798, 2242.820000000000164 ) ) ;
#14561 = CARTESIAN_POINT ( 'NONE',  ( 10.28172140950000113, -3641.012291280000227, 2279.551786969999739 ) ) ;
#14562 = DIRECTION ( 'NONE',  ( -1.000000000000000000, 2.330758767201999921E-14, 2.356218894535000080E-14 ) ) ;
#14563 = CARTESIAN_POINT ( 'NONE',  ( 10.36831320286361979, -3660.851200000155586, 2239.167815367206913 ) ) ;
#14564 = DATE_TIME_ROLE ( 'creation_date' ) ;
#14565 = DIRECTION ( 'NONE',  ( -2.343004830739999973E-14, -1.784212334590129905E-30, -1.000000000000000000 ) ) ;
#14566 = CARTESIAN_POINT ( 'NONE',  ( 18.41519309055000164, -3659.504912144000173, 2244.618989493999834 ) ) ;
#14567 = EDGE_LOOP ( 'NONE', ( #16405, #8116, #14472, #18674 ) ) ;
#14568 = LINE ( 'NONE', #11269, #13043 ) ;
#14569 = CYLINDRICAL_SURFACE ( 'NONE', #2354, 2.844800000000091700 ) ;
#14570 = ORIENTED_EDGE ( 'NONE', *, *, #7220, .F. ) ;
#14571 = EDGE_CURVE ( 'NONE', #11834, #10742, #16672, .T. ) ;
#14572 = ORIENTED_EDGE ( 'NONE', *, *, #6816, .F. ) ;
#14573 = VECTOR ( 'NONE', #4401, 1000.000000000000000 ) ;
#14574 = CARTESIAN_POINT ( 'NONE',  ( 140.5954651218877132, -3662.206385911813868, 2249.347528825103836 ) ) ;
#14575 = VERTEX_POINT ( 'NONE', #14929 ) ;
#14576 = ORIENTED_EDGE ( 'NONE', *, *, #19514, .T. ) ;
#14577 = CARTESIAN_POINT ( 'NONE',  ( 12.69999999999999929, -3648.710000000000036, 2268.705139999999574 ) ) ;
#14578 = VERTEX_POINT ( 'NONE', #9752 ) ;
#14579 = ORIENTED_EDGE ( 'NONE', *, *, #5435, .F. ) ;
#14580 = CARTESIAN_POINT ( 'NONE',  ( 64.76999999999999602, -3670.300000000000182, 2289.213099999999940 ) ) ;
#14581 = FACE_OUTER_BOUND ( 'NONE', #21927, .T. ) ;
#14582 = AXIS2_PLACEMENT_3D ( 'NONE', #3338, #17516, #3574 ) ;
#14583 = ORIENTED_EDGE ( 'NONE', *, *, #15419, .T. ) ;
#14584 = DIRECTION ( 'NONE',  ( -0.8660254037817188832, 0.5000000000047110094, 0.000000000000000000 ) ) ;
#14585 = CARTESIAN_POINT ( 'NONE',  ( 7.360523049854252875, -3581.533682375841181, 2246.411846944129593 ) ) ;
#14586 = TOROIDAL_SURFACE ( 'NONE', #12337, 3.606799999999999784, 0.7620000000000000107 ) ;
#14587 = CARTESIAN_POINT ( 'NONE',  ( 19.17699999999999960, -3659.504999999999654, 2239.009999999999764 ) ) ;
#14588 = APPROVAL_STATUS ( 'not_yet_approved' ) ;
#14589 = EDGE_CURVE ( 'NONE', #15032, #10446, #7893, .T. ) ;
#14590 = APPLICATION_CONTEXT ( 'configuration controlled 3d designs of mechanical parts and assemblies' ) ;
#14591 = EDGE_CURVE ( 'NONE', #16048, #13554, #15466, .T. ) ;
#14592 = EDGE_CURVE ( 'NONE', #11974, #15124, #22194, .T. ) ;
#14593 = VERTEX_POINT ( 'NONE', #15154 ) ;
#14594 = DIRECTION ( 'NONE',  ( 0.000000000000000000, 0.000000000000000000, -1.000000000000000000 ) ) ;
#14595 = CARTESIAN_POINT ( 'NONE',  ( 19.17699999999999960, -3659.504999999999654, 2239.771999999999935 ) ) ;
#14596 = EDGE_CURVE ( 'NONE', #15211, #8549, #11705, .T. ) ;
#14597 = DIRECTION ( 'NONE',  ( 2.324635735433000053E-14, 0.000000000000000000, 1.000000000000000000 ) ) ;
#14598 = ORIENTED_EDGE ( 'NONE', *, *, #7505, .F. ) ;
#14599 = CARTESIAN_POINT ( 'NONE',  ( 12.69999999999999929, -3590.289999999999964, 2257.592639999999847 ) ) ;
#14600 = TOROIDAL_SURFACE ( 'NONE', #1109, 3.606799999999999784, 0.7620000000000000107 ) ;
#14601 = LOCAL_TIME ( 17, 37, 43.00000000000000000, #4807 ) ;
#14602 = CARTESIAN_POINT ( 'NONE',  ( 60.73942059830999796, -3544.061999999999898, 2279.618249568000010 ) ) ;
#14603 =( GEOMETRIC_REPRESENTATION_CONTEXT ( 3 ) GLOBAL_UNCERTAINTY_ASSIGNED_CONTEXT ( ( #13003 ) ) GLOBAL_UNIT_ASSIGNED_CONTEXT ( ( #16076, #1430, #10801 ) ) REPRESENTATION_CONTEXT ( 'NONE', 'WORKASPACE' ) );
#14604 = DIRECTION ( 'NONE',  ( 1.000000000000000000, 0.000000000000000000, 0.000000000000000000 ) ) ;
#14605 = EDGE_CURVE ( 'NONE', #9312, #22767, #13054, .T. ) ;
#14606 = DIRECTION ( 'NONE',  ( 2.902585187577999742E-13, 4.457650181899999573E-12, -1.000000000000000000 ) ) ;
#14607 = EDGE_CURVE ( 'NONE', #3620, #4452, #21076, .T. ) ;
#14608 = LINE ( 'NONE', #14840, #17050 ) ;
#14609 = ORIENTED_EDGE ( 'NONE', *, *, #1960, .F. ) ;
#14610 = CARTESIAN_POINT ( 'NONE',  ( 7.387125747152000876, -3657.399152860999493, 2246.630000000000109 ) ) ;
#14611 = FACE_OUTER_BOUND ( 'NONE', #1728, .T. ) ;
#14612 = LINE ( 'NONE', #16584, #6958 ) ;
#14613 = CARTESIAN_POINT ( 'NONE',  ( -8.890000000032001637, -3658.793800000000374, 2245.060313203000078 ) ) ;
#14614 = CARTESIAN_POINT ( 'NONE',  ( 142.5447279057234198, -3543.405519448513587, 2255.010851276078483 ) ) ;
#14615 = DIRECTION ( 'NONE',  ( 0.000000000000000000, 1.000000000000000000, 0.000000000000000000 ) ) ;
#14616 = CARTESIAN_POINT ( 'NONE',  ( 20.62424768829000143, -3544.570000000000164, 2260.600000000000364 ) ) ;
#14617 = ORIENTED_EDGE ( 'NONE', *, *, #8253, .F. ) ;
#14619 = CIRCLE ( 'NONE', #19473, 0.7619999999999987894 ) ;
#14618 = CALENDAR_DATE ( 2026, 26, 10 ) ;
#14620 = ADVANCED_FACE ( 'NONE', ( #4949 ), #22180, .T. ) ;
#14621 = DIRECTION ( 'NONE',  ( 0.000000000000000000, 0.000000000000000000, -1.000000000000000000 ) ) ;
#14622 = LOCAL_TIME ( 17, 37, 43.00000000000000000, #21222 ) ;
#14623 = SECURITY_CLASSIFICATION ( '', '', #10543 ) ;
#14624 = CARTESIAN_POINT ( 'NONE',  ( -12.31900000000000084, -3660.140000000000327, 2247.392000000000280 ) ) ;
#14625 = CALENDAR_DATE ( 2026, 26, 10 ) ;
#14626 = CARTESIAN_POINT ( 'NONE',  ( 127.0000000000000000, -3670.300000000000182, 2239.771999999999935 ) ) ;
#14627 = CARTESIAN_POINT ( 'NONE',  ( 57.14999999999999858, -3670.300000000000182, 2244.547199999999975 ) ) ;
#14628 = AXIS2_PLACEMENT_3D ( 'NONE', #21124, #6719, #22751 ) ;
#14629 = DIRECTION ( 'NONE',  ( 0.000000000000000000, 0.000000000000000000, -1.000000000000000000 ) ) ;
#14630 = ORIENTED_EDGE ( 'NONE', *, *, #13211, .F. ) ;
#14631 = CARTESIAN_POINT ( 'NONE',  ( 56.10057940169000545, -3694.938000000000102, 2275.211350432000472 ) ) ;
#14632 = ORIENTED_EDGE ( 'NONE', *, *, #16443, .F. ) ;
#14633 = CARTESIAN_POINT ( 'NONE',  ( 18.41499999999899728, -3599.497499999999945, 2295.829799999999977 ) ) ;
#14634 = FACE_OUTER_BOUND ( 'NONE', #14546, .T. ) ;
#14635 = ORIENTED_EDGE ( 'NONE', *, *, #11251, .T. ) ;
#14636 = EDGE_CURVE ( 'NONE', #1414, #20799, #2169, .T. ) ;
#14637 = DIRECTION ( 'NONE',  ( -0.8660254037821902839, -0.5000000000038942183, 0.000000000000000000 ) ) ;
#14638 = LOCAL_TIME ( 17, 37, 43.00000000000000000, #10369 ) ;
#14639 = CIRCLE ( 'NONE', #10514, 1.269999999999882334 ) ;
#14640 = VERTEX_POINT ( 'NONE', #15623 ) ;
#14641 = CARTESIAN_POINT ( 'NONE',  ( 142.3546858854725201, -3695.234698869114709, 2255.486744312730025 ) ) ;
#14642 = FACE_OUTER_BOUND ( 'NONE', #21230, .T. ) ;
#14643 = ORIENTED_EDGE ( 'NONE', *, *, #7154, .T. ) ;
#14644 = CIRCLE ( 'NONE', #19503, 2.844799999999999773 ) ;
#14645 = CARTESIAN_POINT ( 'NONE',  ( 137.3238766226560301, -3581.059663267119049, 2249.196894471709129 ) ) ;
#14646 = PRODUCT_DEFINITION_CONTEXT ( 'detailed design', #15302, 'design' ) ;
#14647 = ORIENTED_EDGE ( 'NONE', *, *, #19519, .T. ) ;
#14648 = FACE_OUTER_BOUND ( 'NONE', #22746, .T. ) ;
#14649 = PERSON_AND_ORGANIZATION_ROLE ( 'creator' ) ;
#14650 = APPLIED_DATE_AND_TIME_ASSIGNMENT ( #7870, #15021, ( #1759 ) ) ;
#14651 = CARTESIAN_POINT ( 'NONE',  ( 14.93205397128999934, -3641.276132144000258, 2279.591813953999463 ) ) ;
#14652 = CARTESIAN_POINT ( 'NONE',  ( 136.6529205195000145, -3543.299999999999727, 2254.503999999999905 ) ) ;
#14653 = CARTESIAN_POINT ( 'NONE',  ( 20.32000000000000028, -3695.699999999999818, 2260.600000000000364 ) ) ;
#14654 = CARTESIAN_POINT ( 'NONE',  ( 10.89511648704999836, -3577.289999577000344, 2257.739442794000297 ) ) ;
#14655 = EDGE_CURVE ( 'NONE', #22478, #6888, #22752, .T. ) ;
#14656 = CARTESIAN_POINT ( 'NONE',  ( 138.5749913602858499, -3576.881732504405591, 2249.436484161916269 ) ) ;
#14657 = ORIENTED_EDGE ( 'NONE', *, *, #6520, .F. ) ;
#14658 = DIRECTION ( 'NONE',  ( 0.000000000000000000, -1.000000000000000000, 0.000000000000000000 ) ) ;
#14659 = ADVANCED_FACE ( 'NONE', ( #8355 ), #850, .T. ) ;
#14660 = AXIS2_PLACEMENT_3D ( 'NONE', #7776, #11506, #2386 ) ;
#14661 = DIRECTION ( 'NONE',  ( 1.224646799147353207E-16, 1.000000000000000000, -0.000000000000000000 ) ) ;
#14662 = ORIENTED_EDGE ( 'NONE', *, *, #20404, .F. ) ;
#14663 = CARTESIAN_POINT ( 'NONE',  ( 50.79999999999999716, -3670.300000000000182, 2239.009999999999764 ) ) ;
#14664 = CARTESIAN_POINT ( 'NONE',  ( 136.9568000000001291, -3658.626742952567838, 2255.967039999999997 ) ) ;
#14665 = ORIENTED_EDGE ( 'NONE', *, *, #9768, .F. ) ;
#14666 = CARTESIAN_POINT ( 'NONE',  ( 15.54479926893309027, -3659.597001414151691, 2257.962943127797644 ) ) ;
#14667 = DIRECTION ( 'NONE',  ( 1.000000000000000000, 0.000000000000000000, 0.000000000000000000 ) ) ;
#14668 = ORIENTED_EDGE ( 'NONE', *, *, #22126, .F. ) ;
#14669 = DIRECTION ( 'NONE',  ( -1.000000000000000000, 0.000000000000000000, 0.000000000000000000 ) ) ;
#14670 = DIRECTION ( 'NONE',  ( 0.000000000000000000, -1.000000000000000000, 0.000000000000000000 ) ) ;
#14671 = CARTESIAN_POINT ( 'NONE',  ( 141.5168031146254464, -3581.684176781325277, 2247.047623956332700 ) ) ;
#14672 = ORIENTED_EDGE ( 'NONE', *, *, #8662, .T. ) ;
#14674 = DIRECTION ( 'NONE',  ( 0.000000000000000000, 0.000000000000000000, 1.000000000000000000 ) ) ;
#14673 = CIRCLE ( 'NONE', #14306, 1.269999999999882334 ) ;
#14675 = PERSON_AND_ORGANIZATION_ROLE ( 'creator' ) ;
#14676 = APPLIED_DATE_AND_TIME_ASSIGNMENT ( #2307, #16708, ( #4495 ) ) ;
#14677 = AXIS2_PLACEMENT_3D ( 'NONE', #478, #7403, #14779 ) ;
#14678 = DIRECTION ( 'NONE',  ( -1.000000000000000000, 0.000000000000000000, 0.000000000000000000 ) ) ;
#14679 = DIRECTION ( 'NONE',  ( 0.000000000000000000, -1.000000000000000000, 0.000000000000000000 ) ) ;
#14680 = ORIENTED_EDGE ( 'NONE', *, *, #7583, .F. ) ;
#14681 = DIRECTION ( 'NONE',  ( 0.000000000000000000, 2.331176954593720496E-12, -1.000000000000000000 ) ) ;
#14682 = DIRECTION ( 'NONE',  ( -0.9296367896483511695, 0.3684771897042033451, 0.000000000000000000 ) ) ;
#14683 = ADVANCED_FACE ( 'NONE', ( #13750 ), #21008, .F. ) ;
#14684 = EDGE_LOOP ( 'NONE', ( #5017, #18759, #5938, #10598 ) ) ;
#14685 = EDGE_CURVE ( 'NONE', #819, #20355, #2682, .T. ) ;
#14686 = CIRCLE ( 'NONE', #8321, 2.844800000000091700 ) ;
#14687 = CARTESIAN_POINT ( 'NONE',  ( 138.3419138266048378, -3662.005144841253241, 2249.540250141421438 ) ) ;
#14688 = EDGE_CURVE ( 'NONE', #17829, #3614, #15733, .T. ) ;
#14689 = ORIENTED_EDGE ( 'NONE', *, *, #1529, .F. ) ;
#14690 = AXIS2_PLACEMENT_3D ( 'NONE', #16420, #7627, #9286 ) ;
#14691 = ORIENTED_EDGE ( 'NONE', *, *, #634, .F. ) ;
#14692 = VECTOR ( 'NONE', #16540, 1000.000000000000000 ) ;
#14693 = CIRCLE ( 'NONE', #17297, 2.844799999998995244 ) ;
#14694 = DIRECTION ( 'NONE',  ( 0.000000000000000000, 0.000000000000000000, -1.000000000000000000 ) ) ;
#14695 = ORIENTED_EDGE ( 'NONE', *, *, #4677, .F. ) ;
#14696 = DIRECTION ( 'NONE',  ( 0.000000000000000000, 0.5000000000005969669, -0.8660254037840939834 ) ) ;
#14697 = FACE_OUTER_BOUND ( 'NONE', #22845, .T. ) ;
#14698 = ORIENTED_EDGE ( 'NONE', *, *, #2158, .T. ) ;
#14699 = CYLINDRICAL_SURFACE ( 'NONE', #20091, 0.3810000000000151599 ) ;
#14700 = LINE ( 'NONE', #12820, #13449 ) ;
#14701 = LINE ( 'NONE', #7437, #3113 ) ;
#14702 = ADVANCED_FACE ( 'NONE', ( #6836 ), #12845, .T. ) ;
#14703 = FACE_OUTER_BOUND ( 'NONE', #5323, .T. ) ;
#14704 = CIRCLE ( 'NONE', #22175, 2.844799999999999773 ) ;
#14705 = APPROVAL_STATUS ( 'not_yet_approved' ) ;
#14706 = VERTEX_POINT ( 'NONE', #19365 ) ;
#14707 = CIRCLE ( 'NONE', #6113, 3.606799999998994366 ) ;
#14708 = TOROIDAL_SURFACE ( 'NONE', #482, 3.606799999999999784, 0.7620000000000000107 ) ;
#14709 = CARTESIAN_POINT ( 'NONE',  ( 151.4000000000000057, -3544.570000000000164, 2240.279999999999745 ) ) ;
#14710 = ORIENTED_EDGE ( 'NONE', *, *, #3254, .F. ) ;
#14711 = FACE_OUTER_BOUND ( 'NONE', #21442, .T. ) ;
#14712 = LINE ( 'NONE', #15800, #5760 ) ;
#14713 = ORIENTED_EDGE ( 'NONE', *, *, #20050, .T. ) ;
#14714 = PLANE ( 'NONE',  #242 ) ;
#14715 = EDGE_CURVE ( 'NONE', #12735, #3057, #11079, .T. ) ;
#14716 = AXIS2_PLACEMENT_3D ( 'NONE', #17744, #17626, #8616 ) ;
#14717 = FACE_OUTER_BOUND ( 'NONE', #1457, .T. ) ;
#14718 = DIRECTION ( 'NONE',  ( 0.000000000000000000, 0.000000000000000000, 1.000000000000000000 ) ) ;
#14719 = AXIS2_PLACEMENT_3D ( 'NONE', #14308, #10899, #7390 ) ;
#14720 = CARTESIAN_POINT ( 'NONE',  ( 16.00573853070648767, -3695.700000000083946, 2281.667430734605205 ) ) ;
#14721 = ORIENTED_EDGE ( 'NONE', *, *, #10222, .T. ) ;
#14722 = EDGE_CURVE ( 'NONE', #7066, #7103, #10218, .T. ) ;
#14723 = EDGE_CURVE ( 'NONE', #4922, #6249, #3454, .T. ) ;
#14724 = CARTESIAN_POINT ( 'NONE',  ( 18.17671024882161035, -3657.870959520586439, 2245.673873547450057 ) ) ;
#14725 = VERTEX_POINT ( 'NONE', #9399 ) ;
#14726 = CARTESIAN_POINT ( 'NONE',  ( 147.5974422321679072, -3695.562642951958424, 2259.905235783985518 ) ) ;
#14727 = CARTESIAN_POINT ( 'NONE',  ( 127.0000000000000000, -3568.700000000000273, 2260.600000000000364 ) ) ;
#14728 = VECTOR ( 'NONE', #1928, 1000.000000000000000 ) ;
#14729 = DIRECTION ( 'NONE',  ( 0.000000000000000000, 0.000000000000000000, 1.000000000000000000 ) ) ;
#14730 = CARTESIAN_POINT ( 'NONE',  ( 127.0000000000000000, -3568.700000000000273, 2261.869999999999891 ) ) ;
#14731 = DIRECTION ( 'NONE',  ( -2.324635735433000053E-14, 2.336881798971000105E-14, -1.000000000000000000 ) ) ;
#14732 = ADVANCED_FACE ( 'NONE', ( #3652 ), #9800, .T. ) ;
#14733 = CARTESIAN_POINT ( 'NONE',  ( 7.036241622171066190, -3578.717921621798268, 2244.547188460646794 ) ) ;
#14734 = VERTEX_POINT ( 'NONE', #11261 ) ;
#14735 = CALENDAR_DATE ( 2026, 26, 10 ) ;
#14736 = ORIENTED_EDGE ( 'NONE', *, *, #16840, .F. ) ;
#14737 = CARTESIAN_POINT ( 'NONE',  ( 132.0583097651000060, -3544.202533098000458, 2260.545675974999995 ) ) ;
#14738 = CARTESIAN_POINT ( 'NONE',  ( 139.6999999999999886, -3577.590000000000146, 2272.030000000000200 ) ) ;
#14739 = AXIS2_PLACEMENT_3D ( 'NONE', #8153, #20672, #10130 ) ;
#14740 = ADVANCED_FACE ( 'NONE', ( #2137 ), #14788, .F. ) ;
#14741 = DIRECTION ( 'NONE',  ( 0.000000000000000000, 0.000000000000000000, 1.000000000000000000 ) ) ;
#14742 = DIRECTION ( 'NONE',  ( 0.000000000000000000, 0.000000000000000000, -1.000000000000000000 ) ) ;
#14743 = DIRECTION ( 'NONE',  ( 0.000000000000000000, 0.000000000000000000, 1.000000000000000000 ) ) ;
#14744 = AXIS2_PLACEMENT_3D ( 'NONE', #8921, #7168, #21804 ) ;
#14745 = VERTEX_POINT ( 'NONE', #10916 ) ;
#14746 = DIRECTION ( 'NONE',  ( 0.000000000000000000, -1.000000000000000000, 0.000000000000000000 ) ) ;
#14747 = ORIENTED_EDGE ( 'NONE', *, *, #7835, .T. ) ;
#14748 = DIRECTION ( 'NONE',  ( -1.000000000000000000, 0.000000000000000000, 0.000000000000000000 ) ) ;
#14749 = EDGE_CURVE ( 'NONE', #14916, #15211, #12809, .T. ) ;
#14750 = CARTESIAN_POINT ( 'NONE',  ( 60.73942059830999796, -3694.938000000000102, 2279.618249568000010 ) ) ;
#14751 = ORIENTED_EDGE ( 'NONE', *, *, #11693, .T. ) ;
#14752 = CARTESIAN_POINT ( 'NONE',  ( 12.69999999999999929, -3579.494999999999891, 2239.771999999999935 ) ) ;
#14753 = TOROIDAL_SURFACE ( 'NONE', #8761, 3.606799999999999784, 0.7620000000000000107 ) ;
#14754 = FACE_OUTER_BOUND ( 'NONE', #20545, .T. ) ;
#14755 = ORIENTED_EDGE ( 'NONE', *, *, #15425, .T. ) ;
#14756 = DIRECTION ( 'NONE',  ( 2.330758767201999921E-14, 1.000000000000000000, 0.000000000000000000 ) ) ;
#14757 = DIRECTION ( 'NONE',  ( 0.000000000000000000, 0.000000000000000000, -1.000000000000000000 ) ) ;
#14758 = ORIENTED_EDGE ( 'NONE', *, *, #12993, .T. ) ;
#14759 = CARTESIAN_POINT ( 'NONE',  ( 137.5719038287758451, -3581.382881717005603, 2248.706519082991235 ) ) ;
#14760 = EDGE_LOOP ( 'NONE', ( #3177, #13768, #11948, #15756 ) ) ;
#14761 = CARTESIAN_POINT ( 'NONE',  ( 145.2613662610192193, -3580.811168667689344, 2245.321774183717480 ) ) ;
#14762 = SECURITY_CLASSIFICATION_LEVEL ( 'unclassified' ) ;
#14763 = ADVANCED_FACE ( 'NONE', ( #4006 ), #20068, .T. ) ;
#14764 = CARTESIAN_POINT ( 'NONE',  ( 145.3808575608765068, -3578.871194572863715, 2244.547198930070408 ) ) ;
#14765 = DIRECTION ( 'NONE',  ( -0.5000000000007065459, 0.8660254037840305896, 0.000000000000000000 ) ) ;
#14766 = TOROIDAL_SURFACE ( 'NONE', #18500, 3.606799999999999784, 0.7620000000000000107 ) ;
#14767 = CARTESIAN_POINT ( 'NONE',  ( 1.270000000000000018, -3544.570000000000164, 2239.009999999999764 ) ) ;
#14768 = VECTOR ( 'NONE', #2652, 1000.000000000000114 ) ;
#14769 = FACE_OUTER_BOUND ( 'NONE', #1744, .T. ) ;
#14770 = AXIS2_PLACEMENT_3D ( 'NONE', #21865, #19773, #5826 ) ;
#14771 = CARTESIAN_POINT ( 'NONE',  ( 138.6135835479743434, -3576.865461055983360, 2249.420587708207222 ) ) ;
#14772 = ORIENTED_EDGE ( 'NONE', *, *, #3541, .T. ) ;
#14773 = DIRECTION ( 'NONE',  ( 1.000000000000000000, 0.000000000000000000, 0.000000000000000000 ) ) ;
#14774 = ORIENTED_EDGE ( 'NONE', *, *, #9360, .T. ) ;
#14775 = CARTESIAN_POINT ( 'NONE',  ( 0.000000000000000000, -3544.061999999999898, 2280.589800000000196 ) ) ;
#14776 = CARTESIAN_POINT ( 'NONE',  ( 15.28733791996542735, -3543.933445093964110, 2255.655544454380106 ) ) ;
#14777 = APPLIED_DATE_AND_TIME_ASSIGNMENT ( #14276, #10401, ( #43 ) ) ;
#14778 = ORIENTED_EDGE ( 'NONE', *, *, #3509, .T. ) ;
#14779 = DIRECTION ( 'NONE',  ( -1.000000000000000000, 0.000000000000000000, 0.000000000000000000 ) ) ;
#14780 = CIRCLE ( 'NONE', #21523, 0.7619999999999294005 ) ;
#14781 = CARTESIAN_POINT ( 'NONE',  ( 135.5205845993333185, -3581.600849088022642, 2246.630007010045119 ) ) ;
#14782 = VECTOR ( 'NONE', #9543, 1000.000000000000114 ) ;
#14783 = ORIENTED_EDGE ( 'NONE', *, *, #3770, .F. ) ;
#14784 = AXIS2_PLACEMENT_3D ( 'NONE', #7561, #21745, #3928 ) ;
#14785 = DIRECTION ( 'NONE',  ( -1.000000000000000000, 0.000000000000000000, 0.000000000000000000 ) ) ;
#14786 = CARTESIAN_POINT ( 'NONE',  ( 12.22806302161694347, -3576.688821853146237, 2249.230233872227018 ) ) ;
#14787 = SHAPE_REPRESENTATION_RELATIONSHIP ( 'NONE' , 'NONE' ,  #19840, #1231 ) ;
#14788 = CYLINDRICAL_SURFACE ( 'NONE', #7992, 2.844800000000001550 ) ;
#14789 = ORIENTED_EDGE ( 'NONE', *, *, #11427, .F. ) ;
#14790 = CARTESIAN_POINT ( 'NONE',  ( 139.3249801263867482, -3662.331213455543548, 2257.597441011418596 ) ) ;
#14791 = PERSON_AND_ORGANIZATION ( #5446, #1895 ) ;
#14792 = CARTESIAN_POINT ( 'NONE',  ( 9.855200508358999301, -3659.504986005999854, 2257.962940201000038 ) ) ;
#14793 = DIRECTION ( 'NONE',  ( 0.000000000000000000, 0.000000000000000000, -1.000000000000000000 ) ) ;
#14794 = ORIENTED_EDGE ( 'NONE', *, *, #1830, .F. ) ;
#14795 = CARTESIAN_POINT ( 'NONE',  ( -12.31900000000002393, -3661.486200000138069, 2245.060313203176065 ) ) ;
#14796 = CARTESIAN_POINT ( 'NONE',  ( 130.6067999999989979, -3568.700000000000273, 2259.837999999999738 ) ) ;
#14797 = AXIS2_PLACEMENT_3D ( 'NONE', #2325, #7170, #13099 ) ;
#14798 = ORIENTED_EDGE ( 'NONE', *, *, #18689, .T. ) ;
#14799 = VECTOR ( 'NONE', #9385, 1000.000000000000000 ) ;
#14800 = CARTESIAN_POINT ( 'NONE',  ( 138.8666558583366566, -3662.225077533978492, 2249.327302760020757 ) ) ;
#14801 = VECTOR ( 'NONE', #1619, 1000.000000000000000 ) ;
#14802 = AXIS2_PLACEMENT_3D ( 'NONE', #16190, #9160, #142 ) ;
#14803 = EDGE_LOOP ( 'NONE', ( #8146, #19491, #19951, #16165 ) ) ;
#14804 = DIRECTION ( 'NONE',  ( 0.000000000000000000, 1.000000000000000000, 0.000000000000000000 ) ) ;
#14805 = APPLIED_PERSON_AND_ORGANIZATION_ASSIGNMENT ( #6613, #13503, ( #11230 ) ) ;
#14806 = CARTESIAN_POINT ( 'NONE',  ( 139.6999999999999886, -3579.494999999999891, 2272.030000000000200 ) ) ;
#14807 = ADVANCED_FACE ( 'NONE', ( #12563, #11154, #2017 ), #18294, .T. ) ;
#14808 = ORIENTED_EDGE ( 'NONE', *, *, #22463, .T. ) ;
#14809 = CARTESIAN_POINT ( 'NONE',  ( 12.69999999999999929, -3599.497499999999945, 2296.210799999999836 ) ) ;
#14810 = APPROVAL_DATE_TIME ( #7538, #5473 ) ;
#14811 = DIRECTION ( 'NONE',  ( 0.000000000000000000, 0.000000000000000000, 1.000000000000000000 ) ) ;
#14812 = EDGE_LOOP ( 'NONE', ( #16416, #19904, #9742, #23041 ) ) ;
#14813 = DIRECTION ( 'NONE',  ( 0.000000000000000000, 0.000000000000000000, -1.000000000000000000 ) ) ;
#14814 = EDGE_CURVE ( 'NONE', #13805, #16994, #2247, .T. ) ;
#14815 =( NAMED_UNIT ( * ) SI_UNIT ( $, .STERADIAN. ) SOLID_ANGLE_UNIT ( ) );
#14816 = CARTESIAN_POINT ( 'NONE',  ( 7.144342338834939632, -3580.833646875532850, 2245.342901023110699 ) ) ;
#14817 = EDGE_CURVE ( 'NONE', #2318, #2712, #16196, .T. ) ;
#14818 = AXIS2_PLACEMENT_3D ( 'NONE', #1719, #22909, #8631 ) ;
#14819 = PERSON_AND_ORGANIZATION ( #5446, #1895 ) ;
#14820 = EDGE_CURVE ( 'NONE', #19266, #4559, #4942, .T. ) ;
#14821 = AXIS2_PLACEMENT_3D ( 'NONE', #20046, #8910, #7157 ) ;
#14822 = AXIS2_PLACEMENT_3D ( 'NONE', #445, #104, #14748 ) ;
#14823 = CARTESIAN_POINT ( 'NONE',  ( 142.2400000000000091, -3580.776127254000130, 2255.774000000000342 ) ) ;
#14824 = VERTEX_POINT ( 'NONE', #18067 ) ;
#14825 = CARTESIAN_POINT ( 'NONE',  ( 142.4504371321982887, -3658.772581173975141, 2249.888537610986077 ) ) ;
#14826 = CARTESIAN_POINT ( 'NONE',  ( 0.000000000000000000, -3544.061999999999898, 2275.763800000000174 ) ) ;
#14827 = ADVANCED_FACE ( 'NONE', ( #9168 ), #5893, .F. ) ;
#14828 = ORIENTED_EDGE ( 'NONE', *, *, #17721, .T. ) ;
#14829 = CARTESIAN_POINT ( 'NONE',  ( 139.6999999999986528, -3582.187400000082107, 2239.391000000000076 ) ) ;
#14830 = CIRCLE ( 'NONE', #7716, 2.844800000000091700 ) ;
#14831 = EDGE_CURVE ( 'NONE', #4249, #19682, #6828, .T. ) ;
#14832 = VECTOR ( 'NONE', #10597, 1000.000000000000000 ) ;
#14833 = LINE ( 'NONE', #20216, #10658 ) ;
#14834 = DIRECTION ( 'NONE',  ( 0.000000000000000000, 0.000000000000000000, -1.000000000000000000 ) ) ;
#14835 = AXIS2_PLACEMENT_3D ( 'NONE', #5321, #12466, #3552 ) ;
#14836 = CARTESIAN_POINT ( 'NONE',  ( 141.9722846279592261, -3581.245981629550442, 2257.824198831835020 ) ) ;
#14837 = PRODUCT_DEFINITION_SHAPE ( 'NONE', 'NONE',  #23165 ) ;
#14838 = EDGE_CURVE ( 'NONE', #12726, #17006, #11665, .T. ) ;
#14839 = CIRCLE ( 'NONE', #18568, 2.844799999999994444 ) ;
#14840 = CARTESIAN_POINT ( 'NONE',  ( 151.1299999999999955, -3694.430000000000291, 2260.600000000000364 ) ) ;
#14841 = ORIENTED_EDGE ( 'NONE', *, *, #3083, .F. ) ;
#14842 = DIRECTION ( 'NONE',  ( 1.224646799147353207E-16, 1.000000000000000000, -0.000000000000000000 ) ) ;
#14843 = CARTESIAN_POINT ( 'NONE',  ( 98.75520000000000209, -3619.500000000000000, 2239.771999999999935 ) ) ;
#14844 = CARTESIAN_POINT ( 'NONE',  ( 9.525000000092171959, -3544.061999999999898, 2281.351800000095409 ) ) ;
#14845 = CIRCLE ( 'NONE', #4729, 0.7619999999999294005 ) ;
#14846 = CARTESIAN_POINT ( 'NONE',  ( 12.69999999999999929, -3576.320000000000164, 2270.760000000000218 ) ) ;
#14847 = CARTESIAN_POINT ( 'NONE',  ( 142.3029786115121453, -3543.951823054115266, 2255.616427089806621 ) ) ;
#14848 = AXIS2_PLACEMENT_3D ( 'NONE', #8481, #10223, #1434 ) ;
#14849 = DIRECTION ( 'NONE',  ( 0.000000000000000000, 0.000000000000000000, -1.000000000000000000 ) ) ;
#14850 = DIRECTION ( 'NONE',  ( 1.000000000000000000, 0.000000000000000000, 0.000000000000000000 ) ) ;
#14851 = VERTEX_POINT ( 'NONE', #21700 ) ;
#14852 = APPLICATION_PROTOCOL_DEFINITION ( 'international standard', 'automotive_design', 2000, #9320 ) ;
#14853 = EDGE_CURVE ( 'NONE', #20079, #7817, #19979, .T. ) ;
#14854 = DIRECTION ( 'NONE',  ( -1.224646799147353207E-16, 1.000000000000000000, 0.000000000000000000 ) ) ;
#14855 = EDGE_CURVE ( 'NONE', #1443, #15832, #17634, .T. ) ;
#14856 = CYLINDRICAL_SURFACE ( 'NONE', #9081, 2.844799999998995244 ) ;
#14857 = VECTOR ( 'NONE', #1925, 1000.000000000000000 ) ;
#14858 = CYLINDRICAL_SURFACE ( 'NONE', #8989, 2.844800000000091700 ) ;
#14859 = AXIS2_PLACEMENT_3D ( 'NONE', #14653, #2229, #16510 ) ;
#14860 = ORIENTED_EDGE ( 'NONE', *, *, #10984, .T. ) ;
#14861 = CARTESIAN_POINT ( 'NONE',  ( 139.6999999999999886, -3659.504999999999654, 2270.760000000000218 ) ) ;
#14862 = ORIENTED_EDGE ( 'NONE', *, *, #22015, .T. ) ;
#14863 = EDGE_LOOP ( 'NONE', ( #17027, #2925 ) ) ;
#14864 = CARTESIAN_POINT ( 'NONE',  ( 14.11996008720290874, -3661.970800930585483, 2249.569598517611666 ) ) ;
#14865 = DIRECTION ( 'NONE',  ( 0.000000000000000000, 0.000000000000000000, 1.000000000000000000 ) ) ;
#14866 = ORIENTED_EDGE ( 'NONE', *, *, #13235, .F. ) ;
#14867 = FACE_OUTER_BOUND ( 'NONE', #17772, .T. ) ;
#14868 = CIRCLE ( 'NONE', #10749, 0.7619999999999294005 ) ;
#14869 = DIRECTION ( 'NONE',  ( 0.000000000000000000, 1.206582004152999850E-12, -1.000000000000000000 ) ) ;
#14870 = VECTOR ( 'NONE', #15497, 1000.000000000000000 ) ;
#14871 = ORIENTED_EDGE ( 'NONE', *, *, #9797, .F. ) ;
#14872 = CARTESIAN_POINT ( 'NONE',  ( 116.8400000000000034, -3695.699999999999818, 2251.506800000000112 ) ) ;
#14873 = DIRECTION ( 'NONE',  ( 0.8660254037817188832, 0.5000000000047110094, -3.192239903041070306E-14 ) ) ;
#14874 = ORIENTED_EDGE ( 'NONE', *, *, #2965, .T. ) ;
#14875 = ORIENTED_EDGE ( 'NONE', *, *, #11707, .F. ) ;
#14876 = VECTOR ( 'NONE', #4460, 1000.000000000000000 ) ;
#14877 = CARTESIAN_POINT ( 'NONE',  ( 136.9873132028999976, -3581.061170452877832, 2239.009999999999764 ) ) ;
#14878 = VERTEX_POINT ( 'NONE', #4456 ) ;
#14879 = CARTESIAN_POINT ( 'NONE',  ( 145.3458854616064286, -3580.386202657235117, 2244.987819353762006 ) ) ;
#14880 = PERSON_AND_ORGANIZATION_ROLE ( 'creator' ) ;
#14881 = EDGE_CURVE ( 'NONE', #15845, #22597, #6882, .T. ) ;
#14882 = ADVANCED_FACE ( 'NONE', ( #17681 ), #17453, .T. ) ;
#14883 = ADVANCED_FACE ( 'NONE', ( #4804 ), #10310, .T. ) ;
#14884 = CARTESIAN_POINT ( 'NONE',  ( 14.21033034659000016, -3641.920435225999881, 2279.715679318999719 ) ) ;
#14885 = EDGE_CURVE ( 'NONE', #19933, #3991, #12187, .T. ) ;
#14886 = CARTESIAN_POINT ( 'NONE',  ( 18.17520605051544891, -3661.148255213616721, 2244.728530265969766 ) ) ;
#14887 = FACE_OUTER_BOUND ( 'NONE', #10708, .T. ) ;
#14888 = CARTESIAN_POINT ( 'NONE',  ( 10.49453184709999931, -3577.690682589000062, 2257.813182895999944 ) ) ;
#14889 = CIRCLE ( 'NONE', #3631, 1.270000000000000240 ) ;
#14890 = CARTESIAN_POINT ( 'NONE',  ( 141.5683389801453416, -3577.348789367103109, 2249.802649695933724 ) ) ;
#14891 = EDGE_CURVE ( 'NONE', #21069, #21998, #8436, .T. ) ;
#14892 = VERTEX_POINT ( 'NONE', #13721 ) ;
#14893 = AXIS2_PLACEMENT_3D ( 'NONE', #7697, #2540, #21992 ) ;
#14894 = ORIENTED_EDGE ( 'NONE', *, *, #5955, .T. ) ;
#14895 = DIRECTION ( 'NONE',  ( 0.000000000000000000, -1.000000000000000000, 1.319970543219000025E-14 ) ) ;
#14896 = VERTEX_POINT ( 'NONE', #6696 ) ;
#14897 = DIRECTION ( 'NONE',  ( 0.000000000000000000, 0.000000000000000000, -1.000000000000000000 ) ) ;
#14898 = DIRECTION ( 'NONE',  ( 0.000000000000000000, 1.000000000000000000, 0.000000000000000000 ) ) ;
#14899 = ADVANCED_FACE ( 'NONE', ( #11952 ), #10544, .T. ) ;
#14900 = EDGE_CURVE ( 'NONE', #15991, #9312, #20651, .T. ) ;
#14901 = ORIENTED_EDGE ( 'NONE', *, *, #17903, .F. ) ;
#14902 = CARTESIAN_POINT ( 'NONE',  ( 141.6126318482000102, -3581.600863517000107, 2246.630000000000109 ) ) ;
#14903 = EDGE_LOOP ( 'NONE', ( #20609, #12810, #19615, #4592 ) ) ;
#14904 = VECTOR ( 'NONE', #18240, 1000.000000000000114 ) ;
#14905 = LINE ( 'NONE', #4346, #5109 ) ;
#14906 = CARTESIAN_POINT ( 'NONE',  ( 15.17514636921737647, -3578.092538392563711, 2250.131376828858265 ) ) ;
#14907 = CARTESIAN_POINT ( 'NONE',  ( 142.4529136091622092, -3580.215257529047449, 2249.894017841437289 ) ) ;
#14908 = ORIENTED_EDGE ( 'NONE', *, *, #16262, .F. ) ;
#14909 = B_SPLINE_CURVE_WITH_KNOTS ( 'NONE', 3,
 ( #1934, #23016, #1700, #12483 ),
 .UNSPECIFIED., .F., .F.,
 ( 4, 4 ),
 ( 0.000000000000000000, 1.000000000000000000 ),
 .UNSPECIFIED. ) ;
#14910 = CARTESIAN_POINT ( 'NONE',  ( 25.39999999999999858, -3578.860000000000127, 2244.547199999999975 ) ) ;
#14911 = PERSON_AND_ORGANIZATION ( #5446, #1895 ) ;
#14912 = CARTESIAN_POINT ( 'NONE',  ( 20.34169023495000062, -3694.797466901999996, 2260.545675974999995 ) ) ;
#14913 = CARTESIAN_POINT ( 'NONE',  ( 38.10000000000000142, -3594.099999999999909, 2259.837999999999738 ) ) ;
#14914 = CARTESIAN_POINT ( 'NONE',  ( 20.79047621426877512, -3543.300000000000637, 2259.421674283870743 ) ) ;
#14915 = DIRECTION ( 'NONE',  ( 0.000000000000000000, 1.000000000000000000, 0.000000000000000000 ) ) ;
#14916 = VERTEX_POINT ( 'NONE', #1515 ) ;
#14917 =( BOUNDED_CURVE ( )  B_SPLINE_CURVE ( 3, ( #15401, #10674, #3086, #1088 ),
 .UNSPECIFIED., .F., .T. ) 
 B_SPLINE_CURVE_WITH_KNOTS ( ( 4, 4 ),
 ( 0.000000000000000000, 1.570796326975000712 ),
 .UNSPECIFIED. ) 
 CURVE ( )  GEOMETRIC_REPRESENTATION_ITEM ( )  RATIONAL_B_SPLINE_CURVE ( ( 1.000000000000000000, 0.8047378540819140058, 0.8047378540819140058, 1.000000000000000000 ) ) 
 REPRESENTATION_ITEM ( '' )  );
#14918 = CARTESIAN_POINT ( 'NONE',  ( 141.8261614683892162, -3661.395196750292598, 2249.944974537677354 ) ) ;
#14919 = ORIENTED_EDGE ( 'NONE', *, *, #1766, .F. ) ;
#14920 = ORIENTED_EDGE ( 'NONE', *, *, #19987, .T. ) ;
#14921 = DIRECTION ( 'NONE',  ( 0.000000000000000000, 0.000000000000000000, -1.000000000000000000 ) ) ;
#14922 = ORIENTED_EDGE ( 'NONE', *, *, #9851, .F. ) ;
#14923 = EDGE_LOOP ( 'NONE', ( #8089, #18466, #3658, #4509 ) ) ;
#14924 = CARTESIAN_POINT ( 'NONE',  ( 9.524999999998000177, -3694.938000000000102, 2281.351799999999912 ) ) ;
#14925 = DIRECTION ( 'NONE',  ( 0.000000000000000000, 0.000000000000000000, 1.000000000000000000 ) ) ;
#14926 = VERTEX_POINT ( 'NONE', #22951 ) ;
#14927 = CARTESIAN_POINT ( 'NONE',  ( 7.269937948888002488, -3657.722882969321745, 2245.891767160526342 ) ) ;
#14928 = FACE_OUTER_BOUND ( 'NONE', #1296, .T. ) ;
#14929 = CARTESIAN_POINT ( 'NONE',  ( 53.64479999999999649, -3670.300000000000182, 2259.837999999999738 ) ) ;
#14930 = CARTESIAN_POINT ( 'NONE',  ( 12.69999999999981988, -3642.677500000000236, 2290.241799999999785 ) ) ;
#14931 = APPLICATION_PROTOCOL_DEFINITION ( 'international standard', 'automotive_design', 2000, #12767 ) ;
#14932 = CYLINDRICAL_SURFACE ( 'NONE', #18767, 0.7619999999999294005 ) ;
#14933 = VERTEX_POINT ( 'NONE', #20979 ) ;
#14934 = APPLIED_PERSON_AND_ORGANIZATION_ASSIGNMENT ( #16989, #11955, ( #20975 ) ) ;
#14935 = DIRECTION ( 'NONE',  ( -0.7071067811866180719, 0.000000000000000000, -0.7071067811864769626 ) ) ;
#14936 = FACE_OUTER_BOUND ( 'NONE', #8782, .T. ) ;
#14937 = ORIENTED_EDGE ( 'NONE', *, *, #3636, .T. ) ;
#14938 = DIRECTION ( 'NONE',  ( 1.000000000000000000, 0.000000000000000000, 0.000000000000000000 ) ) ;
#14939 = EDGE_CURVE ( 'NONE', #12111, #16761, #1630, .T. ) ;
#14940 = ADVANCED_FACE ( 'NONE', ( #8672 ), #13985, .T. ) ;
#14941 = CARTESIAN_POINT ( 'NONE',  ( 14.05634339859000015, -3661.854255679000289, 2239.391000000000076 ) ) ;
#14942 = ORIENTED_EDGE ( 'NONE', *, *, #5973, .T. ) ;
#14943 = CARTESIAN_POINT ( 'NONE',  ( 1.270000000000000018, -3578.860000000000127, 2244.547199999999975 ) ) ;
#14944 = AXIS2_PLACEMENT_3D ( 'NONE', #6405, #13786, #9683 ) ;
#14945 = ADVANCED_FACE ( 'NONE', ( #6918 ), #12307, .T. ) ;
#14946 = DIRECTION ( 'NONE',  ( -1.000000000000000000, 0.000000000000000000, 0.000000000000000000 ) ) ;
#14947 = EDGE_LOOP ( 'NONE', ( #13096, #4627, #7402, #21302 ) ) ;
#14948 = ORIENTED_EDGE ( 'NONE', *, *, #15896, .T. ) ;
#14949 = DIRECTION ( 'NONE',  ( -1.082145837509000041E-12, 1.000000000000000000, 0.000000000000000000 ) ) ;
#14950 = DIRECTION ( 'NONE',  ( 0.000000000000000000, -1.000000000000000000, 0.000000000000000000 ) ) ;
#14951 = CIRCLE ( 'NONE', #4833, 0.7619999999999294005 ) ;
#14952 = FACE_OUTER_BOUND ( 'NONE', #3435, .T. ) ;
#14953 = CARTESIAN_POINT ( 'NONE',  ( 60.21459350834000190, -3695.699999999999818, 2280.170699136999701 ) ) ;
#14954 = DIRECTION ( 'NONE',  ( 0.000000000000000000, 0.000000000000000000, 1.000000000000000000 ) ) ;
#14955 = EDGE_CURVE ( 'NONE', #17874, #13993, #3391, .T. ) ;
#14956 = CARTESIAN_POINT ( 'NONE',  ( 29.00679999999900005, -3568.700000000000273, 2239.771999999999935 ) ) ;
#14957 = DIRECTION ( 'NONE',  ( -1.000000000000000000, 0.000000000000000000, 0.000000000000000000 ) ) ;
#14958 = ORIENTED_EDGE ( 'NONE', *, *, #8169, .F. ) ;
#14959 = APPROVAL_ROLE ( '' ) ;
#14960 = DIRECTION ( 'NONE',  ( 0.000000000000000000, 0.000000000000000000, -1.000000000000000000 ) ) ;
#14961 = FACE_OUTER_BOUND ( 'NONE', #7524, .T. ) ;
#14962 = DIRECTION ( 'NONE',  ( -1.206643234470999950E-12, 1.000000000000000000, 0.000000000000000000 ) ) ;
#14963 = LOCAL_TIME ( 17, 37, 43.00000000000000000, #2721 ) ;
#14964 = AXIS2_PLACEMENT_3D ( 'NONE', #21273, #8848, #1811 ) ;
#14965 = ORIENTED_EDGE ( 'NONE', *, *, #13887, .T. ) ;
#14966 = DIRECTION ( 'NONE',  ( -0.7249994335945011414, -3.300980413455180170E-14, -0.6887494619146010688 ) ) ;
#14967 = ADVANCED_FACE ( 'NONE', ( #22833 ), #3155, .T. ) ;
#14968 = DIRECTION ( 'NONE',  ( -1.000000000000000000, 0.000000000000000000, 0.000000000000000000 ) ) ;
#14969 = ORIENTED_EDGE ( 'NONE', *, *, #3643, .F. ) ;
#14970 = CARTESIAN_POINT ( 'NONE',  ( 127.0000000000000000, -3578.860000000000127, 2244.547199999999975 ) ) ;
#14971 = EDGE_CURVE ( 'NONE', #4732, #20464, #18044, .T. ) ;
#14972 = CARTESIAN_POINT ( 'NONE',  ( 14.45367585492360085, -3661.745009548058079, 2249.740799630053516 ) ) ;
#14973 = EDGE_CURVE ( 'NONE', #10545, #8337, #9450, .T. ) ;
#14974 = CARTESIAN_POINT ( 'NONE',  ( 19.05000000000000071, -3578.860000000000127, 2247.392000000000280 ) ) ;
#14975 = ORIENTED_EDGE ( 'NONE', *, *, #16709, .T. ) ;
#14976 = DIRECTION ( 'NONE',  ( 1.000000000000000000, 0.000000000000000000, 0.000000000000000000 ) ) ;
#14977 = DIRECTION ( 'NONE',  ( 0.000000000000000000, -1.000000000000000000, 0.000000000000000000 ) ) ;
#14978 = ORIENTED_EDGE ( 'NONE', *, *, #17557, .T. ) ;
#14979 = CARTESIAN_POINT ( 'NONE',  ( 10.16000000000000014, -3694.430000000000291, 2255.774000000000342 ) ) ;
#14980 = DIRECTION ( 'NONE',  ( -1.000000000000000000, 0.000000000000000000, 0.000000000000000000 ) ) ;
#14981 = APPLIED_APPROVAL_ASSIGNMENT ( #8051, ( #3363 ) ) ;
#14982 = ORIENTED_EDGE ( 'NONE', *, *, #1540, .F. ) ;
#14983 = EDGE_LOOP ( 'NONE', ( #8328, #4935, #20144, #17537 ) ) ;
#14984 = VECTOR ( 'NONE', #19364, 1000.000000000000114 ) ;
#14985 = DIRECTION ( 'NONE',  ( 0.7249994335945011414, 0.000000000000000000, -0.6887494619146010688 ) ) ;
#14986 = EDGE_CURVE ( 'NONE', #22471, #10418, #15398, .T. ) ;
#14987 = ORIENTED_EDGE ( 'NONE', *, *, #20010, .T. ) ;
#14988 = CARTESIAN_POINT ( 'NONE',  ( 145.1629702012129144, -3581.174070081973241, 2245.736054072267962 ) ) ;
#14989 = SHAPE_DEFINITION_REPRESENTATION ( #8109, #7730 ) ;
#14990 = CARTESIAN_POINT ( 'NONE',  ( 13.92840658401000020, -3642.075073558000440, 2279.750815596999928 ) ) ;
#14991 = CARTESIAN_POINT ( 'NONE',  ( 17.78929153062866320, -3662.104870690277039, 2245.334605559830379 ) ) ;
#14992 = VECTOR ( 'NONE', #7693, 1000.000000000000000 ) ;
#14993 = DIRECTION ( 'NONE',  ( 1.000000000000000000, 2.331176954593550859E-12, 0.000000000000000000 ) ) ;
#14994 = CARTESIAN_POINT ( 'NONE',  ( 151.4000000000000057, -3543.329032635400836, 2260.600000000000364 ) ) ;
#14995 = APPROVAL_PERSON_ORGANIZATION ( #21567, #3604, #10659 ) ;
#14996 = CARTESIAN_POINT ( 'NONE',  ( 137.5725893229727603, -3577.606221452492264, 2249.945671348400538 ) ) ;
#14997 = ORIENTED_EDGE ( 'NONE', *, *, #1771, .T. ) ;
#14998 = APPROVAL_PERSON_ORGANIZATION ( #4379, #12070, #20097 ) ;
#14999 = CARTESIAN_POINT ( 'NONE',  ( -0.7620000000000000107, -3578.860000000000127, 2250.998800000000301 ) ) ;
#15000 = CIRCLE ( 'NONE', #22941, 0.7619999999999294005 ) ;
#15001 = DIRECTION ( 'NONE',  ( 1.000000000000000000, 0.000000000000000000, 0.000000000000000000 ) ) ;
#15002 = ORIENTED_EDGE ( 'NONE', *, *, #2131, .F. ) ;
#15003 = CARTESIAN_POINT ( 'NONE',  ( 3.175000000003000089, -3694.938000000000102, 2275.001800000000003 ) ) ;
#15004 = FACE_OUTER_BOUND ( 'NONE', #3906, .T. ) ;
#15005 = EDGE_CURVE ( 'NONE', #767, #14896, #12049, .T. ) ;
#15006 = EDGE_LOOP ( 'NONE', ( #15261, #1862, #6363, #7876, #7695, #8754, #23029, #5969 ) ) ;
#15007 = AXIS2_PLACEMENT_3D ( 'NONE', #10938, #2271, #20196 ) ;
#15008 = ADVANCED_FACE ( 'NONE', ( #2221 ), #2338, .T. ) ;
#15009 = ORIENTED_EDGE ( 'NONE', *, *, #8303, .F. ) ;
#15010 = VERTEX_POINT ( 'NONE', #7600 ) ;
#15011 = DIRECTION ( 'NONE',  ( 1.000000000000000000, 0.000000000000000000, 0.000000000000000000 ) ) ;
#15012 = ORIENTED_EDGE ( 'NONE', *, *, #3717, .T. ) ;
#15013 = CARTESIAN_POINT ( 'NONE',  ( 12.69999999999999929, -3636.327499999999873, 2264.841800000000148 ) ) ;
#15014 = CARTESIAN_POINT ( 'NONE',  ( 14.97319837854892377, -3577.784037172878925, 2250.025725775317824 ) ) ;
#15015 = APPROVAL_PERSON_ORGANIZATION ( #3949, #16488, #20014 ) ;
#15016 = CARTESIAN_POINT ( 'NONE',  ( 141.7599675853109886, -3581.457171778321481, 2248.553155654074999 ) ) ;
#15017 = EDGE_CURVE ( 'NONE', #8367, #3845, #15433, .T. ) ;
#15018 = ORIENTED_EDGE ( 'NONE', *, *, #7848, .T. ) ;
#15019 = APPLIED_SECURITY_CLASSIFICATION_ASSIGNMENT ( #6775, ( #18354 ) ) ;
#15020 = DIRECTION ( 'NONE',  ( -1.000000000000000000, 0.000000000000000000, 0.000000000000000000 ) ) ;
#15021 = DATE_TIME_ROLE ( 'creation_date' ) ;
#15022 = FACE_OUTER_BOUND ( 'NONE', #10590, .T. ) ;
#15023 = ORIENTED_EDGE ( 'NONE', *, *, #7701, .F. ) ;
#15024 = DIRECTION ( 'NONE',  ( 0.000000000000000000, 0.000000000000000000, -1.000000000000000000 ) ) ;
#15025 = VECTOR ( 'NONE', #1107, 1000.000000000000000 ) ;
#15026 = EDGE_CURVE ( 'NONE', #6791, #9879, #8905, .T. ) ;
#15027 = CARTESIAN_POINT ( 'NONE',  ( 138.2734168420116134, -3577.026766243136080, 2257.683488283899806 ) ) ;
#15028 = VECTOR ( 'NONE', #262, 1000.000000000000000 ) ;
#15029 = EDGE_CURVE ( 'NONE', #22190, #3892, #11007, .T. ) ;
#15030 = ORIENTED_EDGE ( 'NONE', *, *, #22397, .F. ) ;
#15031 = FACE_OUTER_BOUND ( 'NONE', #877, .T. ) ;
#15032 = VERTEX_POINT ( 'NONE', #2331 ) ;
#15033 = VERTEX_POINT ( 'NONE', #6318 ) ;
#15034 = ADVANCED_FACE ( 'NONE', ( #16740 ), #5000, .T. ) ;
#15035 = CARTESIAN_POINT ( 'NONE',  ( 12.69999999999999929, -3590.289999999999964, 2257.592639999999847 ) ) ;
#15036 = ORIENTED_EDGE ( 'NONE', *, *, #1029, .T. ) ;
#15037 = DIRECTION ( 'NONE',  ( 0.000000000000000000, 0.000000000000000000, 1.000000000000000000 ) ) ;
#15038 = DIRECTION ( 'NONE',  ( -0.000000000000000000, -1.000000000000000000, -0.000000000000000000 ) ) ;
#15039 = ORIENTED_EDGE ( 'NONE', *, *, #18364, .F. ) ;
#15040 = AXIS2_PLACEMENT_3D ( 'NONE', #3999, #16304, #2242 ) ;
#15041 = CARTESIAN_POINT ( 'NONE',  ( 7.236841730867277889, -3657.826545604375497, 2245.735190626965050 ) ) ;
#15042 = CARTESIAN_POINT ( 'NONE',  ( 151.4000000000000057, -3695.699999999999818, 2296.591799999999694 ) ) ;
#15043 = DIRECTION ( 'NONE',  ( 1.000000000000000000, -2.330758767201999921E-14, -2.339144844575000061E-14 ) ) ;
#15044 = DIRECTION ( 'NONE',  ( 1.000000000000000000, 0.000000000000000000, 0.000000000000000000 ) ) ;
#15045 = APPROVAL_DATE_TIME ( #7548, #23090 ) ;
#15046 = DIRECTION ( 'NONE',  ( 0.000000000000000000, 0.000000000000000000, 1.000000000000000000 ) ) ;
#15047 = ORIENTED_EDGE ( 'NONE', *, *, #1195, .F. ) ;
#15048 =( BOUNDED_CURVE ( )  B_SPLINE_CURVE ( 3, ( #12817, #289, #18088, #3909 ),
 .UNSPECIFIED., .F., .T. ) 
 B_SPLINE_CURVE_WITH_KNOTS ( ( 4, 4 ),
 ( 1.570796326836454426, 3.141592653589801110 ),
 .UNSPECIFIED. ) 
 CURVE ( )  GEOMETRIC_REPRESENTATION_ITEM ( )  RATIONAL_B_SPLINE_CURVE ( ( 1.000000000000000000, 0.8047378541341584368, 0.8047378541341584368, 1.000000000000000000 ) ) 
 REPRESENTATION_ITEM ( '' )  );
#15049 = EDGE_CURVE ( 'NONE', #6309, #5839, #9922, .T. ) ;
#15050 = DIRECTION ( 'NONE',  ( 1.000000000000000000, 0.000000000000000000, -2.331176954593999892E-13 ) ) ;
#15051 = CARTESIAN_POINT ( 'NONE',  ( 127.0000000000000000, -3578.860000000000127, 2244.547199999999975 ) ) ;
#15052 = VECTOR ( 'NONE', #5167, 1000.000000000000000 ) ;
#15053 = ORIENTED_EDGE ( 'NONE', *, *, #1982, .T. ) ;
#15054 = AXIS2_PLACEMENT_3D ( 'NONE', #3767, #1791, #9051 ) ;
#15055 = CARTESIAN_POINT ( 'NONE',  ( 12.69999999996000106, -3602.189899999999852, 2292.781800000000203 ) ) ;
#15056 = TOROIDAL_SURFACE ( 'NONE', #13171, 4.114799999999999791, 1.270000000000000018 ) ;
#15057 = DIRECTION ( 'NONE',  ( 0.000000000000000000, 1.000000000000000000, 0.000000000000000000 ) ) ;
#15058 = EDGE_LOOP ( 'NONE', ( #12348, #7135, #4023, #21991 ) ) ;
#15059 = CARTESIAN_POINT ( 'NONE',  ( 0.000000000000000000, -3694.430000000000291, 2240.279999999999745 ) ) ;
#15060 = CARTESIAN_POINT ( 'NONE',  ( 18.36215345614126093, -3658.729285337897181, 2244.921339882903339 ) ) ;
#15061 = VERTEX_POINT ( 'NONE', #20260 ) ;
#15062 = VERTEX_POINT ( 'NONE', #20708 ) ;
#15063 = DIRECTION ( 'NONE',  ( 0.000000000000000000, 0.000000000000000000, -1.000000000000000000 ) ) ;
#15064 = VECTOR ( 'NONE', #9897, 1000.000000000000000 ) ;
#15065 = DIRECTION ( 'NONE',  ( -1.000000000000000000, 0.000000000000000000, 0.000000000000000000 ) ) ;
#15066 = DIRECTION ( 'NONE',  ( 1.000000000000000000, -2.334777064353000131E-14, -2.343004830739999973E-14 ) ) ;
#15067 = CARTESIAN_POINT ( 'NONE',  ( 3.048000000000000043, -3543.299999999999727, 2229.612000000000080 ) ) ;
#15068 = CARTESIAN_POINT ( 'NONE',  ( 12.69999999999999929, -3599.497499999999945, 2296.210799999999836 ) ) ;
#15069 = VECTOR ( 'NONE', #6896, 1000.000000000000000 ) ;
#15070 = AXIS2_PLACEMENT_3D ( 'NONE', #14730, #5832, #12967 ) ;
#15071 = CARTESIAN_POINT ( 'NONE',  ( 8.088613972650000150, -3576.119152860999748, 2246.630000000000109 ) ) ;
#15072 = ORIENTED_EDGE ( 'NONE', *, *, #16803, .T. ) ;
#15073 = CALENDAR_DATE ( 2026, 26, 10 ) ;
#15074 = CIRCLE ( 'NONE', #4962, 3.175000000000149925 ) ;
#15075 = DIRECTION ( 'NONE',  ( 0.000000000000000000, 0.000000000000000000, -1.000000000000000000 ) ) ;
#15076 = FACE_BOUND ( 'NONE', #8903, .T. ) ;
#15077 = CARTESIAN_POINT ( 'NONE',  ( 60.73942059830999796, -3544.061999999999898, 2279.618249568000010 ) ) ;
#15078 = ORIENTED_EDGE ( 'NONE', *, *, #13837, .F. ) ;
#15079 = DIRECTION ( 'NONE',  ( 0.000000000000000000, 0.000000000000000000, 1.000000000000000000 ) ) ;
#15080 = B_SPLINE_CURVE_WITH_KNOTS ( 'NONE', 3,
 ( #18509, #5535, #9608, #19932 ),
 .UNSPECIFIED., .F., .F.,
 ( 4, 4 ),
 ( 0.000000000000000000, 1.000000000000000000 ),
 .UNSPECIFIED. ) ;
#15081 = FACE_OUTER_BOUND ( 'NONE', #19269, .T. ) ;
#15082 = CARTESIAN_POINT ( 'NONE',  ( 134.8439533950256930, -3576.481706514296548, 2245.831027411355080 ) ) ;
#15083 = EDGE_LOOP ( 'NONE', ( #2156, #5353, #18077, #7756 ) ) ;
#15084 = CIRCLE ( 'NONE', #4603, 1.269999999999882334 ) ;
#15085 = DIRECTION ( 'NONE',  ( 0.000000000000000000, -1.000000000000000000, 0.000000000000000000 ) ) ;
#15086 = CARTESIAN_POINT ( 'NONE',  ( 137.3683132029000262, -3660.851200000000063, 2239.391000000000076 ) ) ;
#15087 = AXIS2_PLACEMENT_3D ( 'NONE', #5773, #12787, #2015 ) ;
#15088 = CARTESIAN_POINT ( 'NONE',  ( 12.69999999999999929, -3579.494999999999891, 2244.978999999999814 ) ) ;
#15089 = ORIENTED_EDGE ( 'NONE', *, *, #17010, .F. ) ;
#15090 = DIRECTION ( 'NONE',  ( 0.000000000000000000, 0.000000000000000000, 1.000000000000000000 ) ) ;
#15091 = DIRECTION ( 'NONE',  ( -1.000000000000000000, 0.000000000000000000, 0.000000000000000000 ) ) ;
#15092 = APPROVAL ( #12065, 'UNSPECIFIED' ) ;
#15093 = CARTESIAN_POINT ( 'NONE',  ( 12.69999999999999929, -3659.504999999999654, 2246.630000000000109 ) ) ;
#15094 = DIRECTION ( 'NONE',  ( 0.000000000000000000, -1.000000000000000000, 0.000000000000000000 ) ) ;
#15095 = VERTEX_POINT ( 'NONE', #7726 ) ;
#15096 = VECTOR ( 'NONE', #17812, 1000.000000000000000 ) ;
#15097 = ORIENTED_EDGE ( 'NONE', *, *, #15321, .F. ) ;
#15098 = EDGE_CURVE ( 'NONE', #7121, #20865, #22344, .T. ) ;
#15099 = CIRCLE ( 'NONE', #4997, 0.7619999999999294005 ) ;
#15100 = CARTESIAN_POINT ( 'NONE',  ( 15.54479999999999862, -3579.494999999999891, 2272.030000000000200 ) ) ;
#15101 = EDGE_CURVE ( 'NONE', #21296, #1398, #17072, .T. ) ;
#15102 = VERTEX_POINT ( 'NONE', #16958 ) ;
#15104 = CARTESIAN_POINT ( 'NONE',  ( 145.2911534367045192, -3580.678095346821920, 2245.203709730261835 ) ) ;
#15103 = VECTOR ( 'NONE', #18492, 1000.000000000000000 ) ;
#15105 = PERSON_AND_ORGANIZATION ( #3185, #1130 ) ;
#15106 = ADVANCED_FACE ( 'NONE', ( #11678 ), #13216, .T. ) ;
#15107 = CARTESIAN_POINT ( 'NONE',  ( 145.4149999194000316, -3579.495498070999474, 2244.618783703000190 ) ) ;
#15108 = CARTESIAN_POINT ( 'NONE',  ( 17.36210096838674133, -3662.811570847525218, 2246.380819257733037 ) ) ;
#15109 = CARTESIAN_POINT ( 'NONE',  ( 142.1895021644336339, -3580.932314744887208, 2239.010000000037508 ) ) ;
#15110 = CARTESIAN_POINT ( 'NONE',  ( 137.5890733217894706, -3577.587789889484611, 2249.936548038443561 ) ) ;
#15111 = ADVANCED_FACE ( 'NONE', ( #8065 ), #20484, .F. ) ;
#15112 = ORIENTED_EDGE ( 'NONE', *, *, #6732, .T. ) ;
#15113 = AXIS2_PLACEMENT_3D ( 'NONE', #1413, #23078, #22961 ) ;
#15114 = CARTESIAN_POINT ( 'NONE',  ( 7.276091043450246154, -3657.704285925716249, 2245.922240752401649 ) ) ;
#15115 = LINE ( 'NONE', #6214, #7681 ) ;
#15116 = ORIENTED_EDGE ( 'NONE', *, *, #13282, .F. ) ;
#15117 = EDGE_CURVE ( 'NONE', #9417, #20633, #13532, .T. ) ;
#15118 = FACE_OUTER_BOUND ( 'NONE', #9460, .T. ) ;
#15119 = CARTESIAN_POINT ( 'NONE',  ( 10.90808957415271685, -3657.295456685377758, 2247.303068057902237 ) ) ;
#15120 = ORIENTED_EDGE ( 'NONE', *, *, #7128, .F. ) ;
#15121 = ORIENTED_EDGE ( 'NONE', *, *, #17836, .T. ) ;
#15122 = ORIENTED_EDGE ( 'NONE', *, *, #19769, .F. ) ;
#15123 = CARTESIAN_POINT ( 'NONE',  ( 0.7620000000000000107, -3544.061999999999898, 2238.248000000000047 ) ) ;
#15124 = VERTEX_POINT ( 'NONE', #15214 ) ;
#15125 = CARTESIAN_POINT ( 'NONE',  ( 15.03168679714000078, -3598.151299999999992, 2292.781800000000203 ) ) ;
#15126 = CARTESIAN_POINT ( 'NONE',  ( 11.73013214837809848, -3576.819306460322423, 2249.374504195262489 ) ) ;
#15127 = DIRECTION ( 'NONE',  ( 0.000000000000000000, 0.000000000000000000, 1.000000000000000000 ) ) ;
#15128 = CARTESIAN_POINT ( 'NONE',  ( 141.8118641587357160, -3581.401022134622963, 2248.671103578885777 ) ) ;
#15129 = ORIENTED_EDGE ( 'NONE', *, *, #17133, .T. ) ;
#15130 = PLANE ( 'NONE',  #14508 ) ;
#15131 = VECTOR ( 'NONE', #20493, 1000.000000000000000 ) ;
#15132 = APPROVAL_ROLE ( '' ) ;
#15133 = ADVANCED_FACE ( 'NONE', ( #2447 ), #817, .T. ) ;
#15134 = AXIS2_PLACEMENT_3D ( 'NONE', #23033, #17294, #20940 ) ;
#15135 = DIRECTION ( 'NONE',  ( -1.000000000000000000, 0.000000000000000000, 0.000000000000000000 ) ) ;
#15136 = EDGE_CURVE ( 'NONE', #4281, #18259, #13447, .T. ) ;
#15137 = CARTESIAN_POINT ( 'NONE',  ( 137.0026594310930363, -3578.572242505815666, 2257.924723993070984 ) ) ;
#15138 = EDGE_CURVE ( 'NONE', #3669, #159, #18835, .T. ) ;
#15139 = ORIENTED_EDGE ( 'NONE', *, *, #16082, .F. ) ;
#15140 = CARTESIAN_POINT ( 'NONE',  ( 79.04479999999999507, -3670.300000000000182, 2239.771999999999935 ) ) ;
#15141 = ORIENTED_EDGE ( 'NONE', *, *, #19029, .T. ) ;
#15142 = EDGE_LOOP ( 'NONE', ( #12039, #19474, #1614, #14524, #1533, #13460, #7192, #9305, #8828, #13785, #13335 ) ) ;
#15143 = AXIS2_PLACEMENT_3D ( 'NONE', #3233, #17638, #19294 ) ;
#15144 = AXIS2_PLACEMENT_3D ( 'NONE', #8370, #8251, #7278 ) ;
#15145 = CARTESIAN_POINT ( 'NONE',  ( 6.223000000000999066, -3599.497499999999945, 2295.829799999999977 ) ) ;
#15146 = CIRCLE ( 'NONE', #9539, 3.606799999999993567 ) ;
#15147 = ORIENTED_EDGE ( 'NONE', *, *, #5229, .F. ) ;
#15148 = DIRECTION ( 'NONE',  ( 0.000000000000000000, -1.000000000000000000, 4.457650181899999573E-12 ) ) ;
#15149 = DIRECTION ( 'NONE',  ( -0.7071067811865693331, 0.000000000000000000, 0.7071067811865257013 ) ) ;
#15150 = ADVANCED_FACE ( 'NONE', ( #6430 ), #4317, .T. ) ;
#15151 = EDGE_LOOP ( 'NONE', ( #3854, #16736, #15226, #22827 ) ) ;
#15152 = CARTESIAN_POINT ( 'NONE',  ( 7.137204922041744837, -3658.194885328095097, 2245.316081567704714 ) ) ;
#15153 = SHAPE_REPRESENTATION_RELATIONSHIP ( 'NONE' , 'NONE' ,  #1421, #7671 ) ;
#15154 = CARTESIAN_POINT ( 'NONE',  ( 151.1299999999999955, -3544.570000000000164, 2239.009999999999764 ) ) ;
#15155 = CARTESIAN_POINT ( 'NONE',  ( 151.1299999999999955, -3578.860000000000127, 2243.277199999999993 ) ) ;
#15156 = PRODUCT_CONTEXT ( 'NONE', #4076, 'mechanical' ) ;
#15157 = CARTESIAN_POINT ( 'NONE',  ( 0.7620000000000000107, -3695.699999999999818, 2275.763800000000174 ) ) ;
#15158 = LINE ( 'NONE', #18777, #3282 ) ;
#15159 = AXIS2_PLACEMENT_3D ( 'NONE', #20416, #20522, #13046 ) ;
#15160 = CIRCLE ( 'NONE', #2805, 11.11250000000000071 ) ;
#15161 = VECTOR ( 'NONE', #16410, 1000.000000000000000 ) ;
#15163 = CARTESIAN_POINT ( 'NONE',  ( 22.54063073453000143, -3544.061999999999898, 2275.763800000000174 ) ) ;
#15162 = APPLICATION_CONTEXT ( 'configuration controlled 3d designs of mechanical parts and assemblies' ) ;
#15164 = EDGE_CURVE ( 'NONE', #4653, #8438, #9476, .T. ) ;
#15165 = CARTESIAN_POINT ( 'NONE',  ( 1.270000000000000018, -3660.140000000000327, 2247.392000000000280 ) ) ;
#15166 = CIRCLE ( 'NONE', #3570, 5.460999999999938126 ) ;
#15167 = EDGE_LOOP ( 'NONE', ( #3798, #21862, #14920, #21049 ) ) ;
#15168 = CARTESIAN_POINT ( 'NONE',  ( 136.8826269810293468, -3543.437357048151625, 2255.079208148982161 ) ) ;
#15169 = ORIENTED_EDGE ( 'NONE', *, *, #8648, .T. ) ;
#15170 = CARTESIAN_POINT ( 'NONE',  ( 142.4524393039733354, -3580.238099177690401, 2257.938841366922134 ) ) ;
#15171 = LINE ( 'NONE', #6045, #11402 ) ;
#15172 = ORIENTED_EDGE ( 'NONE', *, *, #7774, .F. ) ;
#15173 = EDGE_LOOP ( 'NONE', ( #17928, #11429, #7727, #7786 ) ) ;
#15174 = LINE ( 'NONE', #2975, #22479 ) ;
#15175 = AXIS2_PLACEMENT_3D ( 'NONE', #6600, #13739, #11856 ) ;
#15176 = FACE_OUTER_BOUND ( 'NONE', #4743, .T. ) ;
#15177 = ADVANCED_FACE ( 'NONE', ( #4430 ), #2665, .T. ) ;
#15178 = CIRCLE ( 'NONE', #5079, 2.844800000000091700 ) ;
#15179 = CYLINDRICAL_SURFACE ( 'NONE', #5492, 1.269999999999898099 ) ;
#15180 = EDGE_CURVE ( 'NONE', #3518, #10484, #19182, .T. ) ;
#15181 = FACE_OUTER_BOUND ( 'NONE', #15151, .T. ) ;
#15182 = AXIS2_PLACEMENT_3D ( 'NONE', #4792, #19868, #1388 ) ;
#15183 = CARTESIAN_POINT ( 'NONE',  ( 101.5999999999999943, -3568.700000000000273, 2239.009999999999764 ) ) ;
#15184 = CARTESIAN_POINT ( 'NONE',  ( 88.90000000000000568, -3644.899999999999636, 2260.600000000000364 ) ) ;
#15185 = AXIS2_PLACEMENT_3D ( 'NONE', #4932, #5287, #23080 ) ;
#15186 = ORIENTED_EDGE ( 'NONE', *, *, #10070, .F. ) ;
#15187 = APPROVAL_DATE_TIME ( #9454, #4352 ) ;
#15188 = EDGE_LOOP ( 'NONE', ( #21469, #11731, #4798, #3361 ) ) ;
#15189 = DIRECTION ( 'NONE',  ( -1.000000000000000000, 0.000000000000000000, 0.000000000000000000 ) ) ;
#15190 = DIRECTION ( 'NONE',  ( 0.000000000000000000, -1.000000000000000000, 0.000000000000000000 ) ) ;
#15191 = CARTESIAN_POINT ( 'NONE',  ( 12.69999999999999929, -3659.504999999999654, 2270.760000000000218 ) ) ;
#15192 = AXIS2_PLACEMENT_3D ( 'NONE', #13072, #14729, #427 ) ;
#15193 = ORIENTED_EDGE ( 'NONE', *, *, #20041, .F. ) ;
#15194 = VECTOR ( 'NONE', #4642, 1000.000000000000114 ) ;
#15195 = CARTESIAN_POINT ( 'NONE',  ( 22.55520000000100111, -3568.700000000000273, 2239.771999999999935 ) ) ;
#15196 = VECTOR ( 'NONE', #1608, 1000.000000000000000 ) ;
#15197 = DIRECTION ( 'NONE',  ( 0.000000000000000000, 0.000000000000000000, -1.000000000000000000 ) ) ;
#15198 = DIRECTION ( 'NONE',  ( 1.000000000000000000, 0.000000000000000000, -2.336881798971000105E-14 ) ) ;
#15199 = ORIENTED_EDGE ( 'NONE', *, *, #6061, .T. ) ;
#15200 = CARTESIAN_POINT ( 'NONE',  ( 15.54479999999932716, -3579.043785370524802, 2256.063560000000962 ) ) ;
#15201 = AXIS2_PLACEMENT_3D ( 'NONE', #10258, #1002, #22435 ) ;
#15202 = CARTESIAN_POINT ( 'NONE',  ( 14.93865131287260084, -3661.261308499835195, 2250.006918105073510 ) ) ;
#15203 = CARTESIAN_POINT ( 'NONE',  ( 139.6999999999999886, -3570.287499999999909, 2257.592639999999847 ) ) ;
#15204 = AXIS2_PLACEMENT_3D ( 'NONE', #1159, #4802, #17450 ) ;
#15205 = ORIENTED_EDGE ( 'NONE', *, *, #837, .F. ) ;
#15206 = CARTESIAN_POINT ( 'NONE',  ( -8.890000000008999592, -3662.832400000000234, 2247.392000000000280 ) ) ;
#15207 = LINE ( 'NONE', #22336, #3577 ) ;
#15208 = CARTESIAN_POINT ( 'NONE',  ( 9.855201422231997910, -3599.497499926000273, 2279.447341858000073 ) ) ;
#15209 = CARTESIAN_POINT ( 'NONE',  ( 139.6999999999999886, -3582.670000000000073, 2270.760000000000218 ) ) ;
#15210 = B_SPLINE_CURVE_WITH_KNOTS ( 'NONE', 3,
 ( #12417, #1752, #7042, #3499, #9135 ),
 .UNSPECIFIED., .F., .F.,
 ( 4, 1, 4 ),
 ( 0.000000000000000000, 0.5000000000000000000, 1.000000000000000000 ),
 .UNSPECIFIED. ) ;
#15211 = VERTEX_POINT ( 'NONE', #4890 ) ;
#15212 = ORIENTED_EDGE ( 'NONE', *, *, #18020, .F. ) ;
#15213 = CIRCLE ( 'NONE', #3600, 0.3809999999999647002 ) ;
#15214 = CARTESIAN_POINT ( 'NONE',  ( 144.7800000000000011, -3579.494999999999891, 2245.359999999999673 ) ) ;
#15215 = ORIENTED_EDGE ( 'NONE', *, *, #3482, .F. ) ;
#15216 = AXIS2_PLACEMENT_3D ( 'NONE', #12315, #18157, #5635 ) ;
#15217 = CARTESIAN_POINT ( 'NONE',  ( 145.0360689528194484, -3581.542328872695180, 2246.419514930312289 ) ) ;
#15218 = ITEM_DEFINED_TRANSFORMATION ( 'NONE', 'NONE', #18711,  #5611 ) ;
#15219 = FACE_OUTER_BOUND ( 'NONE', #15266, .T. ) ;
#15220 = CARTESIAN_POINT ( 'NONE',  ( 17.56415751376727741, -3662.505169287860099, 2245.811216528392379 ) ) ;
#15221 = CARTESIAN_POINT ( 'NONE',  ( 20.32000000000000028, -3578.860000000000127, 2247.392000000000280 ) ) ;
#15222 = APPROVAL ( #14588, 'UNSPECIFIED' ) ;
#15223 = DIRECTION ( 'NONE',  ( -1.000000000000000000, 0.000000000000000000, 0.000000000000000000 ) ) ;
#15224 = ADVANCED_FACE ( 'NONE', ( #10162 ), #14323, .T. ) ;
#15225 = DIRECTION ( 'NONE',  ( -0.5000000000007168710, 0.8660254037840248165, 0.000000000000000000 ) ) ;
#15226 = ORIENTED_EDGE ( 'NONE', *, *, #21178, .T. ) ;
#15227 = CARTESIAN_POINT ( 'NONE',  ( 151.1299999999999955, -3660.140000000000327, 2251.506800000000112 ) ) ;
#15228 = TOROIDAL_SURFACE ( 'NONE', #23077, 5.080000000000000071, 0.3810000000000000053 ) ;
#15229 = EDGE_CURVE ( 'NONE', #19560, #7880, #8537, .T. ) ;
#15230 = CARTESIAN_POINT ( 'NONE',  ( 12.69999999999999929, -3590.289999999999964, 2268.705139999999574 ) ) ;
#15231 = VERTEX_POINT ( 'NONE', #1251 ) ;
#15232 = EDGE_CURVE ( 'NONE', #523, #3526, #5480, .T. ) ;
#15233 = FACE_OUTER_BOUND ( 'NONE', #3804, .T. ) ;
#15234 = ADVANCED_BREP_SHAPE_REPRESENTATION ( '', ( #5838, #5611 ), #14218 ) ;
#15235 = AXIS2_PLACEMENT_3D ( 'NONE', #4663, #1025, #20597 ) ;
#15236 = CARTESIAN_POINT ( 'NONE',  ( 142.2400000000000091, -3658.223872745999870, 2255.774000000000342 ) ) ;
#15237 = ADVANCED_FACE ( 'NONE', ( #15442 ), #8327, .T. ) ;
#15238 = VERTEX_POINT ( 'NONE', #8643 ) ;
#15239 = VERTEX_POINT ( 'NONE', #22575 ) ;
#15240 = FACE_OUTER_BOUND ( 'NONE', #5155, .T. ) ;
#15241 = CIRCLE ( 'NONE', #17469, 2.844799999999009010 ) ;
#15242 = ORIENTED_EDGE ( 'NONE', *, *, #17018, .T. ) ;
#15243 = CARTESIAN_POINT ( 'NONE',  ( 85.29320000000001301, -3644.899999999999636, 2259.837999999999738 ) ) ;
#15244 = CARTESIAN_POINT ( 'NONE',  ( 10.88249034213936994, -3577.304564350549299, 2249.774856120668119 ) ) ;
#15245 = CARTESIAN_POINT ( 'NONE',  ( 0.000000000000000000, 0.000000000000000000, 0.000000000000000000 ) ) ;
#15246 = EDGE_CURVE ( 'NONE', #4022, #9982, #9086, .T. ) ;
#15247 = DIRECTION ( 'NONE',  ( 1.000000000000000000, 0.000000000000000000, 0.000000000000000000 ) ) ;
#15248 = ORIENTED_EDGE ( 'NONE', *, *, #16471, .F. ) ;
#15249 = CARTESIAN_POINT ( 'NONE',  ( 137.1443556617770980, -3660.768426910471135, 2257.890254649414146 ) ) ;
#15250 = DATE_AND_TIME ( #8331, #22805 ) ;
#15251 = CIRCLE ( 'NONE', #13746, 0.7619999999999294005 ) ;
#15252 = DIRECTION ( 'NONE',  ( -2.356218894535439317E-14, 0.000000000000000000, -1.000000000000000000 ) ) ;
#15253 = DIRECTION ( 'NONE',  ( 0.000000000000000000, -1.000000000000000000, 0.000000000000000000 ) ) ;
#15254 = EDGE_CURVE ( 'NONE', #4127, #6665, #22919, .T. ) ;
#15255 = TOROIDAL_SURFACE ( 'NONE', #17113, 3.606799999998999695, 0.7620000000000000107 ) ;
#15256 = CARTESIAN_POINT ( 'NONE',  ( 146.1770000000009873, -3579.494999999999891, 2239.771999999999935 ) ) ;
#15257 = AXIS2_PLACEMENT_3D ( 'NONE', #8107, #22839, #15252 ) ;
#15258 = VERTEX_POINT ( 'NONE', #13684 ) ;
#15259 = DIRECTION ( 'NONE',  ( -2.324635735433000053E-14, 0.000000000000000000, -1.000000000000000000 ) ) ;
#15260 = ORIENTED_EDGE ( 'NONE', *, *, #12562, .F. ) ;
#15261 = ORIENTED_EDGE ( 'NONE', *, *, #8263, .T. ) ;
#15262 = ADVANCED_FACE ( 'NONE', ( #17302 ), #10190, .T. ) ;
#15263 = ADVANCED_FACE ( 'NONE', ( #21306 ), #14038, .T. ) ;
#15264 = AXIS2_PLACEMENT_3D ( 'NONE', #17138, #22520, #13508 ) ;
#15265 = DIRECTION ( 'NONE',  ( 0.000000000000000000, 0.000000000000000000, -1.000000000000000000 ) ) ;
#15266 = EDGE_LOOP ( 'NONE', ( #11761, #6111, #21798, #17512 ) ) ;
#15267 = CARTESIAN_POINT ( 'NONE',  ( 3.048000000000000043, -3544.061999999999898, 2228.849999999999909 ) ) ;
#15268 = DIRECTION ( 'NONE',  ( 1.000000000000000000, 2.331176954593550859E-12, 0.000000000000000000 ) ) ;
#15269 = ORIENTED_EDGE ( 'NONE', *, *, #3420, .T. ) ;
#15270 = VECTOR ( 'NONE', #15943, 1000.000000000000000 ) ;
#15271 = FACE_OUTER_BOUND ( 'NONE', #4315, .T. ) ;
#15272 = DIRECTION ( 'NONE',  ( 0.000000000000000000, 0.000000000000000000, -1.000000000000000000 ) ) ;
#15273 = DIRECTION ( 'NONE',  ( 0.000000000000000000, 0.000000000000000000, 1.000000000000000000 ) ) ;
#15274 = PERSON_AND_ORGANIZATION_ROLE ( 'design_supplier' ) ;
#15275 = CARTESIAN_POINT ( 'NONE',  ( 136.8552000000009912, -3579.494999999999891, 2272.030000000000200 ) ) ;
#15276 = CYLINDRICAL_SURFACE ( 'NONE', #3805, 2.844799999999009010 ) ;
#15277 = DIRECTION ( 'NONE',  ( 0.000000000000000000, 1.000000000000000000, 0.000000000000000000 ) ) ;
#15278 = ADVANCED_FACE ( 'NONE', ( #12157 ), #1373, .F. ) ;
#15279 = CARTESIAN_POINT ( 'NONE',  ( 12.70000000003999929, -3662.197400000000016, 2242.820000000000164 ) ) ;
#15280 = AXIS2_PLACEMENT_3D ( 'NONE', #1058, #6239, #6466 ) ;
#15281 = DIRECTION ( 'NONE',  ( -1.000000000000000000, 0.000000000000000000, 0.000000000000000000 ) ) ;
#15282 = ORIENTED_EDGE ( 'NONE', *, *, #4576, .F. ) ;
#15283 = CARTESIAN_POINT ( 'NONE',  ( 137.0372476977747738, -3543.741058433492071, 2255.466570801807393 ) ) ;
#15284 = ORIENTED_EDGE ( 'NONE', *, *, #19174, .F. ) ;
#15285 = VERTEX_POINT ( 'NONE', #8765 ) ;
#15286 = DIRECTION ( 'NONE',  ( 1.000000000000000000, 0.000000000000000000, 0.000000000000000000 ) ) ;
#15287 = CARTESIAN_POINT ( 'NONE',  ( 18.40115537325064210, -3659.045393564460937, 2244.753257970025970 ) ) ;
#15288 = ORIENTED_EDGE ( 'NONE', *, *, #9253, .F. ) ;
#15289 = EDGE_LOOP ( 'NONE', ( #21465, #4475, #21159, #2109 ) ) ;
#15290 = DIRECTION ( 'NONE',  ( 0.000000000000000000, 0.000000000000000000, 1.000000000000000000 ) ) ;
#15291 = DIRECTION ( 'NONE',  ( 0.000000000000000000, 0.000000000000000000, 1.000000000000000000 ) ) ;
#15292 = CARTESIAN_POINT ( 'NONE',  ( 10.12709285722000097, -3600.725217008999607, 2279.515989326000181 ) ) ;
#15293 = EDGE_CURVE ( 'NONE', #2027, #18714, #4958, .T. ) ;
#15294 = CARTESIAN_POINT ( 'NONE',  ( 3.810000000000000053, -3694.938000000000102, 2229.612000000000080 ) ) ;
#15295 = LINE ( 'NONE', #4624, #7230 ) ;
#15296 = EDGE_CURVE ( 'NONE', #2826, #16505, #20307, .T. ) ;
#15297 = LINE ( 'NONE', #17273, #19972 ) ;
#15298 = TOROIDAL_SURFACE ( 'NONE', #10814, 3.606799999999999784, 0.7620000000000000107 ) ;
#15299 = CARTESIAN_POINT ( 'NONE',  ( 9.987313202947046165, -3641.068670452640163, 2296.591799999999694 ) ) ;
#15300 = ORIENTED_EDGE ( 'NONE', *, *, #17396, .T. ) ;
#15301 = CALENDAR_DATE ( 2026, 26, 10 ) ;
#15302 = APPLICATION_CONTEXT ( 'configuration controlled 3d designs of mechanical parts and assemblies' ) ;
#15303 = ORIENTED_EDGE ( 'NONE', *, *, #23023, .F. ) ;
#15304 = FACE_OUTER_BOUND ( 'NONE', #7748, .T. ) ;
#15305 = EDGE_CURVE ( 'NONE', #13470, #7997, #7019, .T. ) ;
#15306 = DIRECTION ( 'NONE',  ( 0.000000000000000000, 0.000000000000000000, -1.000000000000000000 ) ) ;
#15307 = EDGE_LOOP ( 'NONE', ( #3549, #6149, #18741, #2747 ) ) ;
#15308 = ADVANCED_FACE ( 'NONE', ( #19311 ), #2904, .T. ) ;
#15309 = DIRECTION ( 'NONE',  ( -1.000000000000000000, 0.000000000000000000, 0.000000000000000000 ) ) ;
#15310 = EDGE_CURVE ( 'NONE', #21039, #9518, #16515, .T. ) ;
#15311 = CARTESIAN_POINT ( 'NONE',  ( 12.70000000002640661, -3656.812599999840131, 2239.167815367326057 ) ) ;
#15312 = CARTESIAN_POINT ( 'NONE',  ( 144.5381749684807744, -3662.547005267768327, 2245.875428656603162 ) ) ;
#15313 = VERTEX_POINT ( 'NONE', #9115 ) ;
#15314 = AXIS2_PLACEMENT_3D ( 'NONE', #538, #15066, #2193 ) ;
#15315 = DIRECTION ( 'NONE',  ( 2.324635735433000053E-14, 0.000000000000000000, 1.000000000000000000 ) ) ;
#15316 = DIRECTION ( 'NONE',  ( 0.000000000000000000, -1.000000000000000000, 0.000000000000000000 ) ) ;
#15317 = DIRECTION ( 'NONE',  ( 0.000000000000000000, -1.000000000000000000, 0.000000000000000000 ) ) ;
#15318 = EDGE_LOOP ( 'NONE', ( #18198, #9174, #9489, #11245 ) ) ;
#15319 = DIRECTION ( 'NONE',  ( 0.000000000000000000, 0.000000000000000000, -1.000000000000000000 ) ) ;
#15320 = DIRECTION ( 'NONE',  ( -1.622664945668000106E-12, -1.000000000000000000, 0.000000000000000000 ) ) ;
#15321 = EDGE_CURVE ( 'NONE', #9155, #3316, #5680, .T. ) ;
#15322 = CARTESIAN_POINT ( 'NONE',  ( 12.69999999999999929, -3599.497499999999945, 2295.829799999999977 ) ) ;
#15323 = CARTESIAN_POINT ( 'NONE',  ( 14.05634339859000015, -3581.844255679000071, 2239.391000000000076 ) ) ;
#15324 = FACE_OUTER_BOUND ( 'NONE', #22345, .T. ) ;
#15325 = ORIENTED_EDGE ( 'NONE', *, *, #13156, .T. ) ;
#15326 = ORIENTED_EDGE ( 'NONE', *, *, #4840, .T. ) ;
#15327 = CIRCLE ( 'NONE', #18318, 2.844800000000091700 ) ;
#15328 = CARTESIAN_POINT ( 'NONE',  ( 19.05000000000000071, -3660.140000000000327, 2247.392000000000280 ) ) ;
#15329 = ORIENTED_EDGE ( 'NONE', *, *, #6427, .T. ) ;
#15330 = CARTESIAN_POINT ( 'NONE',  ( 12.70000020906999971, -3582.339800010000090, 2257.592639999999847 ) ) ;
#15331 = DATE_TIME_ROLE ( 'classification_date' ) ;
#15332 = DIRECTION ( 'NONE',  ( 1.122008997397786234E-13, 0.000000000000000000, 1.000000000000000000 ) ) ;
#15333 = CARTESIAN_POINT ( 'NONE',  ( 142.3985385445537872, -3578.575513665826293, 2257.925021594871851 ) ) ;
#15334 = DIRECTION ( 'NONE',  ( 2.336881798971000105E-14, 2.336881798971000105E-14, 1.000000000000000000 ) ) ;
#15335 = FACE_OUTER_BOUND ( 'NONE', #22118, .T. ) ;
#15336 = CARTESIAN_POINT ( 'NONE',  ( 9.652920519510999497, -3695.699999999999818, 2254.503999999999905 ) ) ;
#15337 = DIRECTION ( 'NONE',  ( 0.8660254037817188832, 0.5000000000047110094, -3.192239903041070306E-14 ) ) ;
#15338 = ORIENTED_EDGE ( 'NONE', *, *, #10684, .F. ) ;
#15339 = TOROIDAL_SURFACE ( 'NONE', #16096, 3.606799999998999695, 0.7620000000000000107 ) ;
#15340 = DIRECTION ( 'NONE',  ( 0.000000000000000000, 0.000000000000000000, -1.000000000000000000 ) ) ;
#15341 = DIRECTION ( 'NONE',  ( 5.432398939370942693E-28, 1.000000000000000000, 2.336881798971000105E-14 ) ) ;
#15342 = VERTEX_POINT ( 'NONE', #12738 ) ;
#15343 = LOCAL_TIME ( 17, 37, 43.00000000000000000, #4459 ) ;
#15344 = CARTESIAN_POINT ( 'NONE',  ( 12.69999999999999929, -3659.504999999999654, 2246.630000000000109 ) ) ;
#15345 = CARTESIAN_POINT ( 'NONE',  ( 10.57779571310348565, -3657.610496412460179, 2248.693734300258257 ) ) ;
#15346 = ORIENTED_EDGE ( 'NONE', *, *, #20749, .T. ) ;
#15347 = ORIENTED_EDGE ( 'NONE', *, *, #22284, .T. ) ;
#15348 = VERTEX_POINT ( 'NONE', #10863 ) ;
#15349 = DIRECTION ( 'NONE',  ( 1.000000000000000000, 0.000000000000000000, 0.000000000000000000 ) ) ;
#15350 = ORIENTED_EDGE ( 'NONE', *, *, #22397, .T. ) ;
#15351 = APPLIED_PERSON_AND_ORGANIZATION_ASSIGNMENT ( #19226, #9845, ( #3730 ) ) ;
#15352 = CARTESIAN_POINT ( 'NONE',  ( 76.20000000000000284, -3568.700000000000273, 2260.600000000000364 ) ) ;
#15353 = DIRECTION ( 'NONE',  ( 1.000000000000000000, 0.000000000000000000, 0.000000000000000000 ) ) ;
#15354 = CARTESIAN_POINT ( 'NONE',  ( 0.000000000000000000, 0.000000000000000000, 0.000000000000000000 ) ) ;
#15355 = CARTESIAN_POINT ( 'NONE',  ( 142.4352164564301688, -3580.278531256406040, 2249.858390971456629 ) ) ;
#15356 = ORIENTED_EDGE ( 'NONE', *, *, #12385, .T. ) ;
#15357 = DIRECTION ( 'NONE',  ( 0.7249994335945011414, 0.000000000000000000, 0.6887494619146010688 ) ) ;
#15358 = DATE_TIME_ROLE ( 'classification_date' ) ;
#15359 = AXIS2_PLACEMENT_3D ( 'NONE', #13343, #17427, #19078 ) ;
#15360 = EDGE_CURVE ( 'NONE', #20085, #19933, #1276, .T. ) ;
#15361 = LINE ( 'NONE', #11718, #21988 ) ;
#15362 = APPLIED_APPROVAL_ASSIGNMENT ( #6053, ( #16481 ) ) ;
#15363 = CARTESIAN_POINT ( 'NONE',  ( 129.8447999999989975, -3619.500000000000000, 2261.869999999999891 ) ) ;
#15364 = APPLIED_APPROVAL_ASSIGNMENT ( #20655, ( #5365 ) ) ;
#15365 = EDGE_CURVE ( 'NONE', #1958, #7536, #16680, .T. ) ;
#15366 = CARTESIAN_POINT ( 'NONE',  ( 134.2006755046125761, -3657.949543878901750, 2245.576349614068477 ) ) ;
#15367 = CIRCLE ( 'NONE', #19859, 0.7619999999999554907 ) ;
#15368 = EDGE_LOOP ( 'NONE', ( #1269, #788, #17610, #16315 ) ) ;
#15369 = CARTESIAN_POINT ( 'NONE',  ( 12.69999999999999929, -3659.504999999999654, 2239.391000000000076 ) ) ;
#15370 = ORIENTED_EDGE ( 'NONE', *, *, #18162, .T. ) ;
#15371 = LINE ( 'NONE', #13613, #11346 ) ;
#15372 = DIRECTION ( 'NONE',  ( 0.000000000000000000, 0.000000000000000000, -1.000000000000000000 ) ) ;
#15373 = EDGE_LOOP ( 'NONE', ( #5204, #22165, #16128, #5794 ) ) ;
#15374 = APPROVAL_PERSON_ORGANIZATION ( #21308, #1885, #23045 ) ;
#15375 = DIRECTION ( 'NONE',  ( -1.169647906252999915E-12, 1.000000000000000000, 0.000000000000000000 ) ) ;
#15376 = DIRECTION ( 'NONE',  ( 0.000000000000000000, 0.000000000000000000, 1.000000000000000000 ) ) ;
#15377 = APPROVAL_PERSON_ORGANIZATION ( #6031, #11350, #2507 ) ;
#15378 = VERTEX_POINT ( 'NONE', #20012 ) ;
#15379 = APPLIED_PERSON_AND_ORGANIZATION_ASSIGNMENT ( #16595, #7920, ( #10933 ) ) ;
#15380 = DIRECTION ( 'NONE',  ( 0.7071067811865969777, 0.000000000000000000, 0.7071067811864980568 ) ) ;
#15381 = CARTESIAN_POINT ( 'NONE',  ( 12.69999999999999929, -3655.060000000000400, 2268.705139999999574 ) ) ;
#15382 = FACE_OUTER_BOUND ( 'NONE', #2248, .T. ) ;
#15383 = SHAPE_DEFINITION_REPRESENTATION ( #3002, #15665 ) ;
#15384 = AXIS2_PLACEMENT_3D ( 'NONE', #7455, #18229, #5939 ) ;
#15385 = ADVANCED_FACE ( 'NONE', ( #7357 ), #10980, .F. ) ;
#15386 = DIRECTION ( 'NONE',  ( 0.000000000000000000, 1.000000000000000000, 0.000000000000000000 ) ) ;
#15387 = LINE ( 'NONE', #19138, #2324 ) ;
#15388 = VERTEX_POINT ( 'NONE', #207 ) ;
#15389 = CARTESIAN_POINT ( 'NONE',  ( 152.4000000000000057, -3694.938000000000102, 2275.763800000000174 ) ) ;
#15390 = EDGE_CURVE ( 'NONE', #22006, #13646, #3034, .T. ) ;
#15391 = EDGE_CURVE ( 'NONE', #17959, #9684, #10902, .T. ) ;
#15392 = CARTESIAN_POINT ( 'NONE',  ( 12.69999999999999929, -3653.027999999999793, 2274.293139999999767 ) ) ;
#15393 = FACE_OUTER_BOUND ( 'NONE', #5592, .T. ) ;
#15394 = SECURITY_CLASSIFICATION ( '', '', #10825 ) ;
#15395 = ORIENTED_EDGE ( 'NONE', *, *, #4070, .F. ) ;
#15396 = CARTESIAN_POINT ( 'NONE',  ( 15.03168679714000078, -3640.848700000000008, 2292.781800000000203 ) ) ;
#15397 = ORIENTED_EDGE ( 'NONE', *, *, #22996, .T. ) ;
#15398 = B_SPLINE_CURVE_WITH_KNOTS ( 'NONE', 3,
 ( #5041, #12419, #3503, #10654, #17804, #8326, #14298, #17916, #2, #16050, #2111, #7380, #117, #11004, #12649, #7487, #21443, #7150, #5519, #19800, #10773, #9257, #18038, #14645, #1756, #5393, #3734, #12531, #19688, #3622, #18148, #19916, #11127, #12763, #14759, #14534, #1868, #12881, #7263, #9020, #16393, #344, #239, #10889, #21671, #3856, #1987, #21785, #456, #5627, #14412, #16166, #9139, #5747, #9368, #16279, #20034 ),
 .UNSPECIFIED., .F., .F.,
 ( 4, 2, 2, 1, 1, 2, 2, 2, 2, 1, 1, 1, 2, 2, 2, 2, 2, 2, 1, 1, 2, 2, 2, 2, 2, 2, 2, 2, 2, 2, 2, 4 ),
 ( 0.000000000000000000, 0.1249999999985798027, 0.1874999999980038745, 0.2187499999977179366, 0.2343749999975340836, 0.2421874999975122955, 0.2499999999974905074, 0.3124999999980864751, 0.3437499999984656163, 0.3593749999987312926, 0.3671874999987232990, 0.3710937499987121968, 0.3730468749987710386, 0.3749999999988298249, 0.4062499999969994557, 0.4374999999951690866, 0.4687499999933387174, 0.4843749999924235050, 0.4921874999918540161, 0.4960937499915020199, 0.4980468749914571114, 0.4999999999914122029, 0.5624999999926729721, 0.5937499999933033568, 0.6093749999936185491, 0.6249999999939337414, 0.6874999999948844254, 0.7499999999958351093, 0.8124999999967857933, 0.8437499999972610798, 0.8749999999977363663, 1.000000000000000000 ),
 .UNSPECIFIED. ) ;
#15399 = EDGE_LOOP ( 'NONE', ( #21264, #11780, #8078, #5014 ) ) ;
#15400 = CIRCLE ( 'NONE', #6041, 0.3809999999999647002 ) ;
#15401 = CARTESIAN_POINT ( 'NONE',  ( 3.175000000094025054, -3694.938000000000102, 2275.001800000090952 ) ) ;
#15402 = AXIS2_PLACEMENT_3D ( 'NONE', #1426, #12327, #19471 ) ;
#15403 = DIRECTION ( 'NONE',  ( 0.000000000000000000, 0.000000000000000000, 1.000000000000000000 ) ) ;
#15404 = ORIENTED_EDGE ( 'NONE', *, *, #16255, .F. ) ;
#15405 = ORIENTED_EDGE ( 'NONE', *, *, #8801, .F. ) ;
#15406 = LINE ( 'NONE', #11416, #7164 ) ;
#15407 = EDGE_CURVE ( 'NONE', #8713, #6183, #20626, .T. ) ;
#15408 = DIRECTION ( 'NONE',  ( 5.572969907074833723E-14, -1.000000000000000000, 0.000000000000000000 ) ) ;
#15409 = DIRECTION ( 'NONE',  ( 0.000000000000000000, 0.000000000000000000, -1.000000000000000000 ) ) ;
#15410 = ORIENTED_EDGE ( 'NONE', *, *, #5302, .T. ) ;
#15411 = CARTESIAN_POINT ( 'NONE',  ( 12.69999999999999929, -3579.494999999999891, 2244.978999999999814 ) ) ;
#15412 = CARTESIAN_POINT ( 'NONE',  ( 142.5448000000000093, -3579.494999999999891, 2256.063560000000052 ) ) ;
#15413 = LINE ( 'NONE', #4858, #21104 ) ;
#15414 = CARTESIAN_POINT ( 'NONE',  ( 20.71779849188069633, -3695.670697890124757, 2259.603314403323111 ) ) ;
#15415 = VERTEX_POINT ( 'NONE', #16480 ) ;
#15416 = APPROVAL_STATUS ( 'not_yet_approved' ) ;
#15417 = ORIENTED_EDGE ( 'NONE', *, *, #2965, .F. ) ;
#15418 = CIRCLE ( 'NONE', #5319, 5.460999999999938126 ) ;
#15419 = EDGE_CURVE ( 'NONE', #13988, #8337, #13142, .T. ) ;
#15420 = AXIS2_PLACEMENT_3D ( 'NONE', #3729, #11002, #1984 ) ;
#15421 = CARTESIAN_POINT ( 'NONE',  ( 10.90591201611552918, -3581.702760788150499, 2247.525194624931828 ) ) ;
#15422 = DIRECTION ( 'NONE',  ( 0.000000000000000000, 1.000000000000000000, 0.000000000000000000 ) ) ;
#15423 = VERTEX_POINT ( 'NONE', #12629 ) ;
#15424 = DIRECTION ( 'NONE',  ( -1.000000000000000000, 0.000000000000000000, 0.000000000000000000 ) ) ;
#15425 = EDGE_CURVE ( 'NONE', #13523, #16613, #19894, .T. ) ;
#15426 = ADVANCED_FACE ( 'NONE', ( #9230 ), #16143, .T. ) ;
#15427 = CARTESIAN_POINT ( 'NONE',  ( 3.048000000000000043, -3694.938000000000102, 2229.612000000000080 ) ) ;
#15428 = CARTESIAN_POINT ( 'NONE',  ( 144.9794953955964445, -3661.698965784566099, 2245.005495991907537 ) ) ;
#15429 = CARTESIAN_POINT ( 'NONE',  ( 12.70000000023333264, -3602.629840905158289, 2296.591799999999694 ) ) ;
#15430 = CARTESIAN_POINT ( 'NONE',  ( 10.80273383056147729, -3661.626674884904787, 2249.818717145221399 ) ) ;
#15431 = FACE_OUTER_BOUND ( 'NONE', #18817, .T. ) ;
#15432 = VERTEX_POINT ( 'NONE', #17775 ) ;
#15433 = CIRCLE ( 'NONE', #12860, 5.460999999999938126 ) ;
#15434 = DIRECTION ( 'NONE',  ( -1.000000000000000000, 0.000000000000000000, 0.000000000000000000 ) ) ;
#15435 = CIRCLE ( 'NONE', #9063, 3.606799999999993567 ) ;
#15436 = FACE_OUTER_BOUND ( 'NONE', #6795, .T. ) ;
#15437 = CARTESIAN_POINT ( 'NONE',  ( 22.54063073453000143, -3544.061999999999898, 2275.763800000000174 ) ) ;
#15438 = CARTESIAN_POINT ( 'NONE',  ( 12.07304487791000192, -3596.716615716000433, 2279.801384127999881 ) ) ;
#15439 = CARTESIAN_POINT ( 'NONE',  ( 15.54479951278000094, -3579.494996001999880, 2250.165024905999871 ) ) ;
#15440 = EDGE_CURVE ( 'NONE', #14376, #22036, #586, .T. ) ;
#15441 = VERTEX_POINT ( 'NONE', #10628 ) ;
#15442 = FACE_OUTER_BOUND ( 'NONE', #18863, .T. ) ;
#15443 = ORIENTED_EDGE ( 'NONE', *, *, #21710, .T. ) ;
#15444 = CARTESIAN_POINT ( 'NONE',  ( 9.886192531064313727, -3543.438632178772878, 2255.088321282487868 ) ) ;
#15446 = CIRCLE ( 'NONE', #5351, 0.7619999999999294005 ) ;
#15445 = ITEM_DEFINED_TRANSFORMATION ( 'NONE', 'NONE', #4124,  #5611 ) ;
#15447 = DIRECTION ( 'NONE',  ( -1.000000000000000000, 0.000000000000000000, 0.000000000000000000 ) ) ;
#15448 = DIRECTION ( 'NONE',  ( 0.000000000000000000, 0.000000000000000000, -1.000000000000000000 ) ) ;
#15449 = CARTESIAN_POINT ( 'NONE',  ( 12.15052771711000013, -3662.300804947000415, 2257.605120077999800 ) ) ;
#15450 = VECTOR ( 'NONE', #6395, 999.9999999999998863 ) ;
#15451 = DIRECTION ( 'NONE',  ( 0.000000000000000000, 0.000000000000000000, 1.000000000000000000 ) ) ;
#15452 = CYLINDRICAL_SURFACE ( 'NONE', #3496, 0.3809999999999260090 ) ;
#15453 = AXIS2_PLACEMENT_3D ( 'NONE', #15620, #3417, #19363 ) ;
#15454 = ADVANCED_FACE ( 'NONE', ( #16027 ), #23151, .T. ) ;
#15455 = SPHERICAL_SURFACE ( 'NONE', #18483, 0.7620000000000000107 ) ;
#15456 = VERTEX_POINT ( 'NONE', #21419 ) ;
#15457 = DIRECTION ( 'NONE',  ( 0.8660254037817188832, -0.5000000000047110094, -1.484475890921031808E-12 ) ) ;
#15458 = FACE_OUTER_BOUND ( 'NONE', #10774, .T. ) ;
#15459 = ORIENTED_EDGE ( 'NONE', *, *, #799, .T. ) ;
#15460 = DIRECTION ( 'NONE',  ( -2.185478394939000111E-13, -2.590196616223999907E-13, -1.000000000000000000 ) ) ;
#15461 = CARTESIAN_POINT ( 'NONE',  ( 10.79926234752687364, -3657.388342404155082, 2248.114296700302475 ) ) ;
#15462 = ORIENTED_EDGE ( 'NONE', *, *, #4197, .F. ) ;
#15463 = VERTEX_POINT ( 'NONE', #22091 ) ;
#15464 = CARTESIAN_POINT ( 'NONE',  ( 133.9850000019999925, -3579.713624101472305, 2244.668992692525990 ) ) ;
#15465 = B_SPLINE_CURVE_WITH_KNOTS ( 'NONE', 3,
 ( #18770, #514, #22395, #21950, #728, #13269, #18658, #11289, #13159, #9645, #2717, #16562, #5916, #11396, #13052, #4143, #18433, #843, #2605, #9866, #15152, #4593, #2390, #7891, #17012, #958, #9528, #18545, #7780, #15041, #2503, #11738, #2836, #14927, #16785, #6026, #15114, #17086, #6443, #20379, #13585 ),
 .UNSPECIFIED., .F., .F.,
 ( 4, 2, 2, 1, 1, 2, 2, 2, 2, 1, 1, 1, 2, 2, 2, 2, 2, 2, 2, 1, 1, 2, 2, 4 ),
 ( 0.000000000000000000, 0.1250000000095896624, 0.1875000000141738565, 0.2187500000162666269, 0.2343750000172133141, 0.2421875000176866854, 0.2500000000181600290, 0.3750000000202952655, 0.4375000000211895501, 0.4687500000216366924, 0.4843750000217365570, 0.4921875000216623386, 0.4960937500214908646, 0.5000000000213193907, 0.5625000000132820421, 0.5937500000092633679, 0.6250000000052446936, 0.6874999999972074560, 0.7187499999930718753, 0.7343749999908720794, 0.7421874999900024417, 0.7460937499899599201, 0.7499999999899172876, 1.000000000000000000 ),
 .UNSPECIFIED. ) ;
#15466 = CIRCLE ( 'NONE', #6130, 5.714999999999998082 ) ;
#15467 = EDGE_CURVE ( 'NONE', #23086, #20865, #13191, .T. ) ;
#15468 = EDGE_LOOP ( 'NONE', ( #9471, #19008, #11926, #594 ) ) ;
#15469 = AXIS2_PLACEMENT_3D ( 'NONE', #8223, #4936, #12084 ) ;
#15470 = CARTESIAN_POINT ( 'NONE',  ( 12.69999999996000106, -3602.189899999999852, 2292.781800000000203 ) ) ;
#15471 = CARTESIAN_POINT ( 'NONE',  ( 10.30698504218744382, -3577.956537814648073, 2250.089589229602097 ) ) ;
#15472 = CARTESIAN_POINT ( 'NONE',  ( 0.000000000000000000, 0.000000000000000000, 0.000000000000000000 ) ) ;
#15473 = CARTESIAN_POINT ( 'NONE',  ( 25.39999999999999858, -3660.140000000000327, 2250.236800000000130 ) ) ;
#15474 = ORIENTED_EDGE ( 'NONE', *, *, #132, .F. ) ;
#15475 = CARTESIAN_POINT ( 'NONE',  ( 131.8036441032290895, -3695.561486999931276, 2259.907704032306810 ) ) ;
#15476 = DATE_AND_TIME ( #938, #730 ) ;
#15477 = DIRECTION ( 'NONE',  ( -2.159861190483010203E-14, 0.5000000000030029312, -0.8660254037827048723 ) ) ;
#15478 = CARTESIAN_POINT ( 'NONE',  ( 14.52429522002816675, -3581.677980615632350, 2246.968202618275427 ) ) ;
#15479 = VECTOR ( 'NONE', #8933, 1000.000000000000000 ) ;
#15480 = CARTESIAN_POINT ( 'NONE',  ( 134.3639308053563752, -3657.457671737659439, 2246.419512734921227 ) ) ;
#15481 = EDGE_LOOP ( 'NONE', ( #19142, #22305, #22880, #16866 ) ) ;
#15482 = CARTESIAN_POINT ( 'NONE',  ( 104.4447999999999865, -3670.300000000000182, 2239.771999999999935 ) ) ;
#15483 = APPROVAL ( #14119, 'UNKNOWN' ) ;
#15484 = DIRECTION ( 'NONE',  ( 1.000000000000000000, -2.848812946084999742E-12, 0.000000000000000000 ) ) ;
#15485 = ORIENTED_EDGE ( 'NONE', *, *, #21138, .T. ) ;
#15486 = DIRECTION ( 'NONE',  ( -1.000000000000000000, 0.000000000000000000, 0.000000000000000000 ) ) ;
#15487 = CYLINDRICAL_SURFACE ( 'NONE', #12918, 0.3810000000000011156 ) ;
#15488 = VERTEX_POINT ( 'NONE', #4407 ) ;
#15489 = ORIENTED_EDGE ( 'NONE', *, *, #17536, .F. ) ;
#15490 = CARTESIAN_POINT ( 'NONE',  ( 20.52663075323999919, -3544.443975433000105, 2260.595783961000052 ) ) ;
#15491 = DIRECTION ( 'NONE',  ( 1.000000000000000000, 0.000000000000000000, 0.000000000000000000 ) ) ;
#15492 = VECTOR ( 'NONE', #19903, 1000.000000000000000 ) ;
#15493 = ORIENTED_EDGE ( 'NONE', *, *, #10419, .F. ) ;
#15494 = DIRECTION ( 'NONE',  ( 1.690229834190999937E-12, -1.000000000000000000, 0.000000000000000000 ) ) ;
#15495 = LINE ( 'NONE', #13748, #15941 ) ;
#15496 = CARTESIAN_POINT ( 'NONE',  ( 15.53321004273999861, -3599.811849713999891, 2279.450415087999772 ) ) ;
#15497 = DIRECTION ( 'NONE',  ( 0.000000000000000000, 0.000000000000000000, -1.000000000000000000 ) ) ;
#15498 = COORDINATED_UNIVERSAL_TIME_OFFSET ( 0, 0, .AHEAD. ) ;
#15499 = CARTESIAN_POINT ( 'NONE',  ( 0.000000000000000000, -3544.570000000000164, 2240.279999999999745 ) ) ;
#15500 = DIRECTION ( 'NONE',  ( 0.000000000000000000, -1.000000000000000000, 0.000000000000000000 ) ) ;
#15501 = DIRECTION ( 'NONE',  ( -1.000000000000000000, 0.000000000000000000, 0.000000000000000000 ) ) ;
#15502 = CARTESIAN_POINT ( 'NONE',  ( 141.9552987850744898, -3657.771063528342893, 2248.967151300436399 ) ) ;
#15503 = ORIENTED_EDGE ( 'NONE', *, *, #13727, .F. ) ;
#15504 = AXIS2_PLACEMENT_3D ( 'NONE', #17284, #19521, #10497 ) ;
#15505 = DIRECTION ( 'NONE',  ( 0.8660254037820102058, 0.5000000000042060799, 0.000000000000000000 ) ) ;
#15506 = APPLIED_DATE_AND_TIME_ASSIGNMENT ( #9533, #11869, ( #12786 ) ) ;
#15507 = VECTOR ( 'NONE', #7400, 1000.000000000000000 ) ;
#15508 = CIRCLE ( 'NONE', #5421, 5.460999999999938126 ) ;
#15509 = ORIENTED_EDGE ( 'NONE', *, *, #2896, .T. ) ;
#15510 = CARTESIAN_POINT ( 'NONE',  ( -12.69999999999999929, -3575.727659095000035, 2247.392000000000280 ) ) ;
#15511 = DIRECTION ( 'NONE',  ( 0.000000000000000000, 0.000000000000000000, -1.000000000000000000 ) ) ;
#15512 = EDGE_CURVE ( 'NONE', #21090, #6888, #21764, .T. ) ;
#15513 = ORIENTED_EDGE ( 'NONE', *, *, #3000, .T. ) ;
#15514 = EDGE_LOOP ( 'NONE', ( #1323, #19236, #10415, #18489 ) ) ;
#15515 = DIRECTION ( 'NONE',  ( -1.000000000000000000, 2.330758767201999921E-14, 2.343004830739999973E-14 ) ) ;
#15516 = EDGE_CURVE ( 'NONE', #21672, #16839, #3786, .T. ) ;
#15517 = DIRECTION ( 'NONE',  ( 0.000000000000000000, -1.000000000000000000, 0.000000000000000000 ) ) ;
#15518 = DIRECTION ( 'NONE',  ( 0.7071067811865969777, 0.000000000000000000, 0.7071067811864980568 ) ) ;
#15519 = EDGE_CURVE ( 'NONE', #2778, #10901, #15400, .T. ) ;
#15520 = ORIENTED_EDGE ( 'NONE', *, *, #22157, .F. ) ;
#15521 = CARTESIAN_POINT ( 'NONE',  ( 136.9568000000001291, -3580.373257047432617, 2255.967039999999997 ) ) ;
#15522 = DIRECTION ( 'NONE',  ( 0.000000000000000000, 0.000000000000000000, 1.000000000000000000 ) ) ;
#15523 = CARTESIAN_POINT ( 'NONE',  ( 9.855200508358999301, -3579.494986006000545, 2257.962940201000038 ) ) ;
#15524 = CIRCLE ( 'NONE', #16692, 0.7619999999999294005 ) ;
#15525 = CYLINDRICAL_SURFACE ( 'NONE', #6500, 2.844800000000091700 ) ;
#15526 = CIRCLE ( 'NONE', #556, 5.080000000000000959 ) ;
#15527 = CARTESIAN_POINT ( 'NONE',  ( 57.14999999999999858, -3568.700000000000273, 2247.392000000000280 ) ) ;
#15528 = EDGE_LOOP ( 'NONE', ( #11020, #7343, #7099, #709 ) ) ;
#15529 = DATE_TIME_ROLE ( 'creation_date' ) ;
#15530 = VECTOR ( 'NONE', #1270, 1000.000000000000000 ) ;
#15531 = ORIENTED_EDGE ( 'NONE', *, *, #4938, .F. ) ;
#15532 = AXIS2_PLACEMENT_3D ( 'NONE', #16442, #21499, #19741 ) ;
#15533 = EDGE_CURVE ( 'NONE', #13997, #5890, #22494, .T. ) ;
#15534 = DIRECTION ( 'NONE',  ( 0.000000000000000000, 0.000000000000000000, 1.000000000000000000 ) ) ;
#15535 = CARTESIAN_POINT ( 'NONE',  ( 10.38213137239466732, -3581.144250671618011, 2249.087841259171910 ) ) ;
#15536 = EDGE_CURVE ( 'NONE', #18172, #3458, #11541, .T. ) ;
#15537 = ORIENTED_EDGE ( 'NONE', *, *, #10538, .F. ) ;
#15538 = DIRECTION ( 'NONE',  ( -1.000000000000000000, 0.000000000000000000, 0.000000000000000000 ) ) ;
#15539 = EDGE_CURVE ( 'NONE', #3845, #17805, #9782, .T. ) ;
#15540 = CIRCLE ( 'NONE', #18899, 1.269999999999882334 ) ;
#15541 = CARTESIAN_POINT ( 'NONE',  ( 20.34169023495000062, -3544.202533098000458, 2260.545675974999995 ) ) ;
#15542 = CARTESIAN_POINT ( 'NONE',  ( 145.3794022844519702, -3660.142231666386579, 2244.547199809527683 ) ) ;
#15543 = B_SPLINE_CURVE_WITH_KNOTS ( 'NONE', 3,
 ( #7961, #4327, #11466, #18618 ),
 .UNSPECIFIED., .F., .F.,
 ( 4, 4 ),
 ( 0.9999968116805088014, 1.000000000000000000 ),
 .UNSPECIFIED. ) ;
#15544 = DIRECTION ( 'NONE',  ( 0.000000000000000000, 1.000000000000000000, 0.000000000000000000 ) ) ;
#15545 = CARTESIAN_POINT ( 'NONE',  ( 11.44214827259342293, -3662.056613363663928, 2249.494299770979069 ) ) ;
#15546 = PRODUCT ( 'Magnet Chuck Plate', 'Magnet Chuck Plate', '', ( #10689 ) ) ;
#15547 = TOROIDAL_SURFACE ( 'NONE', #19250, 3.606799999998999695, 0.7620000000000000107 ) ;
#15548 = DIRECTION ( 'NONE',  ( -1.000000000000000000, 0.000000000000000000, 0.000000000000000000 ) ) ;
#15549 = CIRCLE ( 'NONE', #21905, 1.904999999999823501 ) ;
#15550 = ORIENTED_EDGE ( 'NONE', *, *, #21194, .T. ) ;
#15551 = CARTESIAN_POINT ( 'NONE',  ( -12.70000000000011831, -3578.860000000000127, 2242.311999999999898 ) ) ;
#15552 = CARTESIAN_POINT ( 'NONE',  ( 14.93205609083999974, -3637.728870509999979, 2279.591813517999981 ) ) ;
#15553 = EDGE_CURVE ( 'NONE', #3316, #9155, #7540, .T. ) ;
#15554 = CARTESIAN_POINT ( 'NONE',  ( 12.70000000002484875, -3582.187400000083926, 2239.391000000000076 ) ) ;
#15555 = CARTESIAN_POINT ( 'NONE',  ( 10.68380249261999992, -3597.481841244999941, 2279.634034043999691 ) ) ;
#15556 = DIRECTION ( 'NONE',  ( 0.000000000000000000, 0.000000000000000000, 1.000000000000000000 ) ) ;
#15557 = VERTEX_POINT ( 'NONE', #18690 ) ;
#15558 = ORIENTED_EDGE ( 'NONE', *, *, #21141, .F. ) ;
#15559 = CARTESIAN_POINT ( 'NONE',  ( 12.69999999996000106, -3642.634840905000146, 2296.591799999999694 ) ) ;
#15560 = CIRCLE ( 'NONE', #8458, 5.079999999999973426 ) ;
#15561 = ORIENTED_EDGE ( 'NONE', *, *, #15995, .F. ) ;
#15562 = CARTESIAN_POINT ( 'NONE',  ( 12.70000000000085727, -3636.657698770567094, 2279.817639764978139 ) ) ;
#15563 = VECTOR ( 'NONE', #9007, 1000.000000000000000 ) ;
#15564 = SECURITY_CLASSIFICATION_LEVEL ( 'unclassified' ) ;
#15565 = DIRECTION ( 'NONE',  ( -1.000000000000000000, 0.000000000000000000, 0.000000000000000000 ) ) ;
#15566 = CIRCLE ( 'NONE', #18553, 2.844800000000091700 ) ;
#15567 = ORIENTED_EDGE ( 'NONE', *, *, #18670, .F. ) ;
#15568 = AXIS2_PLACEMENT_3D ( 'NONE', #5735, #16268, #21663 ) ;
#15569 = DIRECTION ( 'NONE',  ( 0.000000000000000000, 0.000000000000000000, -1.000000000000000000 ) ) ;
#15570 = CARTESIAN_POINT ( 'NONE',  ( 12.69999999999999929, -3634.041499999999814, 2290.241799999999785 ) ) ;
#15571 = TOROIDAL_SURFACE ( 'NONE', #15201, 3.606799999999999784, 0.7620000000000000107 ) ;
#15572 = DIRECTION ( 'NONE',  ( 1.000000000000000000, 0.000000000000000000, 0.000000000000000000 ) ) ;
#15573 = FACE_OUTER_BOUND ( 'NONE', #20950, .T. ) ;
#15574 = AXIS2_PLACEMENT_3D ( 'NONE', #15243, #22370, #6229 ) ;
#15575 = CIRCLE ( 'NONE', #6968, 1.523999999999858801 ) ;
#15576 = FACE_BOUND ( 'NONE', #329, .T. ) ;
#15577 = VERTEX_POINT ( 'NONE', #22203 ) ;
#15578 = FACE_BOUND ( 'NONE', #16457, .T. ) ;
#15579 = LINE ( 'NONE', #13937, #12553 ) ;
#15580 = ORIENTED_EDGE ( 'NONE', *, *, #20664, .F. ) ;
#15581 = VECTOR ( 'NONE', #16810, 1000.000000000000000 ) ;
#15582 = DIRECTION ( 'NONE',  ( 0.000000000000000000, 1.000000000000000000, 0.000000000000000000 ) ) ;
#15583 = CARTESIAN_POINT ( 'NONE',  ( 147.3230419228115693, -3694.590198012000656, 2260.592443268617444 ) ) ;
#15584 = CIRCLE ( 'NONE', #9178, 2.844800000000091700 ) ;
#15585 = ORIENTED_EDGE ( 'NONE', *, *, #7998, .T. ) ;
#15586 = VECTOR ( 'NONE', #19856, 1000.000000000000000 ) ;
#15587 = ORIENTED_EDGE ( 'NONE', *, *, #3430, .T. ) ;
#15588 = CARTESIAN_POINT ( 'NONE',  ( 76.20000000000000284, -3670.300000000000182, 2259.837999999999738 ) ) ;
#15589 = ORIENTED_EDGE ( 'NONE', *, *, #9526, .T. ) ;
#15590 = EDGE_CURVE ( 'NONE', #19446, #15348, #2309, .T. ) ;
#15591 = DIRECTION ( 'NONE',  ( 2.347365683444999541E-13, 0.000000000000000000, -1.000000000000000000 ) ) ;
#15592 = EDGE_CURVE ( 'NONE', #21188, #14926, #15698, .T. ) ;
#15593 = DIRECTION ( 'NONE',  ( 0.000000000000000000, 0.000000000000000000, 1.000000000000000000 ) ) ;
#15594 = TOROIDAL_SURFACE ( 'NONE', #2129, 4.114799999999999791, 1.270000000000000018 ) ;
#15595 = EDGE_CURVE ( 'NONE', #13823, #18734, #437, .T. ) ;
#15596 = CARTESIAN_POINT ( 'NONE',  ( 9.652920519510999497, -3695.699999999999818, 2254.503999999999905 ) ) ;
#15597 = VERTEX_POINT ( 'NONE', #13080 ) ;
#15598 = CARTESIAN_POINT ( 'NONE',  ( 131.7018716228582491, -3695.661851662454410, 2259.652921219497784 ) ) ;
#15599 = APPROVAL_ROLE ( '' ) ;
#15600 = CARTESIAN_POINT ( 'NONE',  ( 9.956800000000452400, -3578.616742952519417, 2255.967039999999997 ) ) ;
#15601 = DIRECTION ( 'NONE',  ( 1.000000000000000000, 0.000000000000000000, 0.000000000000000000 ) ) ;
#15602 = EDGE_CURVE ( 'NONE', #14578, #13412, #16880, .T. ) ;
#15603 = DIRECTION ( 'NONE',  ( -1.000000000000000000, 0.000000000000000000, 0.000000000000000000 ) ) ;
#15604 = CIRCLE ( 'NONE', #5137, 2.844800000000091700 ) ;
#15605 = DIRECTION ( 'NONE',  ( 0.000000000000000000, 0.000000000000000000, -1.000000000000000000 ) ) ;
#15606 = ORIENTED_EDGE ( 'NONE', *, *, #6520, .T. ) ;
#15607 = TOROIDAL_SURFACE ( 'NONE', #14103, 3.606799999999999784, 0.7620000000000000107 ) ;
#15608 = CARTESIAN_POINT ( 'NONE',  ( 15.56750744765447436, -3695.617810904695034, 2254.953947933142899 ) ) ;
#15609 = EDGE_CURVE ( 'NONE', #16863, #15557, #6062, .T. ) ;
#15610 = ADVANCED_FACE ( 'NONE', ( #18585 ), #2535, .F. ) ;
#15611 = CARTESIAN_POINT ( 'NONE',  ( 3.048000000000000043, -3544.061999999999898, 2239.009999999999764 ) ) ;
#15612 = VERTEX_POINT ( 'NONE', #6400 ) ;
#15613 = CARTESIAN_POINT ( 'NONE',  ( 79.80679999999999552, -3568.700000000000273, 2260.600000000000364 ) ) ;
#15614 = DIRECTION ( 'NONE',  ( -1.000000000000000000, 0.000000000000000000, 0.000000000000000000 ) ) ;
#15615 = VERTEX_POINT ( 'NONE', #17390 ) ;
#15616 = ORIENTED_EDGE ( 'NONE', *, *, #20017, .F. ) ;
#15617 = FACE_OUTER_BOUND ( 'NONE', #8479, .T. ) ;
#15618 = ORIENTED_EDGE ( 'NONE', *, *, #18901, .T. ) ;
#15619 = AXIS2_PLACEMENT_3D ( 'NONE', #16536, #489, #14211 ) ;
#15620 = CARTESIAN_POINT ( 'NONE',  ( 59.89320000000000022, -3644.899999999999636, 2259.837999999999738 ) ) ;
#15621 = CARTESIAN_POINT ( 'NONE',  ( 2.859369265473000077, -3695.699999999999818, 2275.763800000000174 ) ) ;
#15622 =( NAMED_UNIT ( * ) PLANE_ANGLE_UNIT ( ) SI_UNIT ( $, .RADIAN. ) );
#15623 = CARTESIAN_POINT ( 'NONE',  ( 97.99320000000000164, -3568.700000000000273, 2260.600000000000364 ) ) ;
#15624 = DIRECTION ( 'NONE',  ( 0.000000000000000000, 0.000000000000000000, 1.000000000000000000 ) ) ;
#15625 = PERSON_AND_ORGANIZATION_ROLE ( 'classification_officer' ) ;
#15626 = AXIS2_PLACEMENT_3D ( 'NONE', #12636, #17783, #21315 ) ;
#15627 = AXIS2_PLACEMENT_3D ( 'NONE', #16877, #9626, #7871 ) ;
#15628 = CARTESIAN_POINT ( 'NONE',  ( 7.020566483207999475, -3660.139755500999854, 2244.547200037999573 ) ) ;
#15629 = DIRECTION ( 'NONE',  ( 0.000000000000000000, 0.000000000000000000, -1.000000000000000000 ) ) ;
#15630 = CYLINDRICAL_SURFACE ( 'NONE', #7061, 6.349999999999855760 ) ;
#15631 = CIRCLE ( 'NONE', #11498, 1.269999999999882334 ) ;
#15632 = CARTESIAN_POINT ( 'NONE',  ( 142.1880353584854220, -3658.125296333661936, 2249.401294179523120 ) ) ;
#15633 = ORIENTED_EDGE ( 'NONE', *, *, #15592, .T. ) ;
#15634 = CARTESIAN_POINT ( 'NONE',  ( -8.890000000028999594, -3656.101400000000012, 2245.060313203000078 ) ) ;
#15635 = AXIS2_PLACEMENT_3D ( 'NONE', #9231, #16372, #323 ) ;
#15636 = ORIENTED_EDGE ( 'NONE', *, *, #22391, .T. ) ;
#15637 = AXIS2_PLACEMENT_3D ( 'NONE', #15828, #9996, #19025 ) ;
#15638 = CARTESIAN_POINT ( 'NONE',  ( 116.8400000000000034, -3694.430000000000291, 2250.236800000000130 ) ) ;
#15639 = ORIENTED_EDGE ( 'NONE', *, *, #8090, .T. ) ;
#15640 = ORIENTED_EDGE ( 'NONE', *, *, #1197, .T. ) ;
#15641 = CARTESIAN_POINT ( 'NONE',  ( 15.24000000000000021, -3544.570000000000164, 2255.774000000000342 ) ) ;
#15642 = CARTESIAN_POINT ( 'NONE',  ( -8.890000000026999416, -3657.447599999999966, 2247.392000000000280 ) ) ;
#15643 = CARTESIAN_POINT ( 'NONE',  ( 136.8552000000001669, -3659.956214629431997, 2256.063560000000052 ) ) ;
#15644 = ORIENTED_EDGE ( 'NONE', *, *, #19899, .T. ) ;
#15645 = DIRECTION ( 'NONE',  ( 0.000000000000000000, 0.000000000000000000, 1.000000000000000000 ) ) ;
#15646 = FACE_OUTER_BOUND ( 'NONE', #6693, .T. ) ;
#15647 = LINE ( 'NONE', #15763, #21061 ) ;
#15648 = CARTESIAN_POINT ( 'NONE',  ( 12.69999999999999929, -3599.497499999999945, 2263.571799999999712 ) ) ;
#15649 = DIRECTION ( 'NONE',  ( -1.000000000000000000, 0.000000000000000000, 0.000000000000000000 ) ) ;
#15650 = VERTEX_POINT ( 'NONE', #8619 ) ;
#15651 = PERSON_AND_ORGANIZATION_ROLE ( 'creator' ) ;
#15652 = PRODUCT_DEFINITION ( 'UNKNOWN', '', #10864, #17210 ) ;
#15653 = AXIS2_PLACEMENT_3D ( 'NONE', #8456, #22612, #3397 ) ;
#15654 = EDGE_LOOP ( 'NONE', ( #22444, #23039, #16278, #20501 ) ) ;
#15655 = DIRECTION ( 'NONE',  ( 0.000000000000000000, 0.000000000000000000, -1.000000000000000000 ) ) ;
#15656 = CARTESIAN_POINT ( 'NONE',  ( 63.50000000000000000, -3594.099999999999909, 2239.009999999999764 ) ) ;
#15657 = EDGE_CURVE ( 'NONE', #9083, #8878, #5305, .T. ) ;
#15658 = DIRECTION ( 'NONE',  ( -1.000000000000000000, 0.000000000000000000, 0.000000000000000000 ) ) ;
#15659 = EDGE_LOOP ( 'NONE', ( #2600, #11804 ) ) ;
#15660 = ORIENTED_EDGE ( 'NONE', *, *, #9995, .T. ) ;
#15661 = FACE_BOUND ( 'NONE', #5603, .T. ) ;
#15662 = EDGE_CURVE ( 'NONE', #13767, #671, #19080, .T. ) ;
#15663 = CARTESIAN_POINT ( 'NONE',  ( -5.588000000000000078, -3543.299999999999727, 2253.487999999999829 ) ) ;
#15664 = CARTESIAN_POINT ( 'NONE',  ( 144.7333290304783304, -3662.211819972148987, 2245.442509231050281 ) ) ;
#15665 = SHAPE_REPRESENTATION ( 'Screw 2', ( #5611 ), #2257 ) ;
#15666 = DIRECTION ( 'NONE',  ( 0.000000000000000000, 0.000000000000000000, 1.000000000000000000 ) ) ;
#15667 = CYLINDRICAL_SURFACE ( 'NONE', #9201, 2.844800000000091700 ) ;
#15668 = CARTESIAN_POINT ( 'NONE',  ( 147.5076778864620621, -3543.579977980994954, 2260.129759352632391 ) ) ;
#15669 = ORIENTED_EDGE ( 'NONE', *, *, #6163, .F. ) ;
#15670 = CARTESIAN_POINT ( 'NONE',  ( 12.69999999999999929, -3639.502500000000055, 2296.210799999999836 ) ) ;
#15671 = VECTOR ( 'NONE', #13912, 1000.000000000000000 ) ;
#15672 = PLANE ( 'NONE',  #1330 ) ;
#15673 = FACE_OUTER_BOUND ( 'NONE', #14187, .T. ) ;
#15674 = CARTESIAN_POINT ( 'NONE',  ( 12.69999999999999929, -3583.940000000000055, 2275.055139999999483 ) ) ;
#15675 = DIRECTION ( 'NONE',  ( 0.000000000000000000, 0.000000000000000000, 1.000000000000000000 ) ) ;
#15676 = ORIENTED_EDGE ( 'NONE', *, *, #6881, .F. ) ;
#15677 = DIRECTION ( 'NONE',  ( 0.000000000000000000, 0.000000000000000000, -1.000000000000000000 ) ) ;
#15678 = ORIENTED_EDGE ( 'NONE', *, *, #6216, .T. ) ;
#15679 = DIRECTION ( 'NONE',  ( 0.000000000000000000, 0.000000000000000000, -1.000000000000000000 ) ) ;
#15680 = SECURITY_CLASSIFICATION_LEVEL ( 'unclassified' ) ;
#15681 = DIRECTION ( 'NONE',  ( 0.000000000000000000, 0.000000000000000000, -1.000000000000000000 ) ) ;
#15682 = EDGE_CURVE ( 'NONE', #11141, #13004, #12255, .T. ) ;
#15683 = CARTESIAN_POINT ( 'NONE',  ( 15.03168679714000078, -3598.151299999999992, 2292.781800000000203 ) ) ;
#15684 = DIRECTION ( 'NONE',  ( 2.324635735433000053E-14, 0.000000000000000000, 1.000000000000000000 ) ) ;
#15685 = EDGE_CURVE ( 'NONE', #15820, #12468, #10485, .T. ) ;
#15686 = AXIS2_PLACEMENT_3D ( 'NONE', #10973, #5484, #21753 ) ;
#15687 = ADVANCED_FACE ( 'NONE', ( #18929 ), #1168, .T. ) ;
#15688 = CARTESIAN_POINT ( 'NONE',  ( 88.90000000000000568, -3644.899999999999636, 2259.837999999999738 ) ) ;
#15689 = ADVANCED_FACE ( 'NONE', ( #22781 ), #6871, .F. ) ;
#15690 = DIRECTION ( 'NONE',  ( 1.000000000000000000, 0.000000000000000000, 0.000000000000000000 ) ) ;
#15691 = CARTESIAN_POINT ( 'NONE',  ( 139.6999999999999886, -3659.504999999999654, 2244.978999999999814 ) ) ;
#15692 = ORIENTED_EDGE ( 'NONE', *, *, #8354, .T. ) ;
#15693 = CARTESIAN_POINT ( 'NONE',  ( 147.8270794805000037, -3695.699999999999818, 2259.329999999999927 ) ) ;
#15694 = DIRECTION ( 'NONE',  ( 0.000000000000000000, 0.8660254037817070039, -0.5000000000047313264 ) ) ;
#15695 = ORIENTED_EDGE ( 'NONE', *, *, #7361, .T. ) ;
#15696 = DIRECTION ( 'NONE',  ( 0.000000000000000000, -1.000000000000000000, 0.000000000000000000 ) ) ;
#15697 = CARTESIAN_POINT ( 'NONE',  ( 10.46449438243440433, -3657.744798957563944, 2248.928716950800663 ) ) ;
#15698 = B_SPLINE_CURVE_WITH_KNOTS ( 'NONE', 3,
 ( #12973, #6174, #4295, #4175, #873, #9564, #8039, #9457, #16596, #16710, #664, #7691, #13423, #11650, #18807, #17045, #8160, #21874, #5840, #21984, #547 ),
 .UNSPECIFIED., .F., .F.,
 ( 4, 2, 2, 1, 2, 2, 2, 2, 2, 2, 4 ),
 ( 0.000000000000000000, 0.1249999999978197440, 0.1874999999967315034, 0.2187499999964521435, 0.2343749999963124497, 0.2499999999961727837, 0.3749999999969789721, 0.4999999999977851051, 0.7499999999988021804, 0.8749999999994011457, 1.000000000000000000 ),
 .UNSPECIFIED. ) ;
#15699 = CIRCLE ( 'NONE', #22359, 1.269999999999882334 ) ;
#15700 = ORIENTED_EDGE ( 'NONE', *, *, #2856, .T. ) ;
#15701 = DIRECTION ( 'NONE',  ( 1.000000000000000000, 0.000000000000000000, 0.000000000000000000 ) ) ;
#15702 = ADVANCED_FACE ( 'NONE', ( #5110 ), #9032, .T. ) ;
#15703 = ORIENTED_EDGE ( 'NONE', *, *, #19418, .T. ) ;
#15704 = DIRECTION ( 'NONE',  ( 0.000000000000000000, -1.000000000000000000, 0.000000000000000000 ) ) ;
#15705 = DATE_TIME_ROLE ( 'creation_date' ) ;
#15706 = DIRECTION ( 'NONE',  ( -1.000000000000000000, 0.000000000000000000, 0.000000000000000000 ) ) ;
#15707 = VERTEX_POINT ( 'NONE', #3333 ) ;
#15708 = CARTESIAN_POINT ( 'NONE',  ( 137.0014614162122655, -3580.414486297099756, 2257.925021603513869 ) ) ;
#15709 = CALENDAR_DATE ( 2026, 26, 10 ) ;
#15710 = DIRECTION ( 'NONE',  ( -1.224646799147353207E-16, 1.000000000000000000, 0.000000000000000000 ) ) ;
#15711 = CARTESIAN_POINT ( 'NONE',  ( 14.52753400248703741, -3581.675156902885647, 2247.803913149289656 ) ) ;
#15712 = TOROIDAL_SURFACE ( 'NONE', #16459, 3.606799999999999784, 0.7620000000000000107 ) ;
#15713 = EDGE_CURVE ( 'NONE', #819, #4457, #19165, .T. ) ;
#15714 = CARTESIAN_POINT ( 'NONE',  ( 76.20000000000000284, -3568.700000000000273, 2239.771999999999935 ) ) ;
#15715 = APPROVAL_PERSON_ORGANIZATION ( #11717, #12204, #15599 ) ;
#15716 = CARTESIAN_POINT ( 'NONE',  ( 88.90000000000000568, -3594.099999999999909, 2239.771999999999935 ) ) ;
#15717 = ORIENTED_EDGE ( 'NONE', *, *, #23035, .T. ) ;
#15718 = DIRECTION ( 'NONE',  ( 1.000000000000000000, 0.000000000000000000, 0.000000000000000000 ) ) ;
#15719 = EDGE_CURVE ( 'NONE', #1882, #8573, #3104, .T. ) ;
#15720 = ADVANCED_FACE ( 'NONE', ( #15304 ), #12015, .T. ) ;
#15721 = FACE_OUTER_BOUND ( 'NONE', #7081, .T. ) ;
#15722 = ORIENTED_EDGE ( 'NONE', *, *, #7445, .F. ) ;
#15723 = CARTESIAN_POINT ( 'NONE',  ( 136.9873132030508600, -3577.928829547506666, 2239.009999999999764 ) ) ;
#15724 = DIRECTION ( 'NONE',  ( -7.093784530908000077E-13, -1.000000000000000000, -3.793660610171000449E-12 ) ) ;
#15725 = ORIENTED_EDGE ( 'NONE', *, *, #3073, .F. ) ;
#15726 = ORIENTED_EDGE ( 'NONE', *, *, #3765, .T. ) ;
#15727 = CARTESIAN_POINT ( 'NONE',  ( 137.3683132029000262, -3580.841199999999844, 2242.820000000000164 ) ) ;
#15728 = DIRECTION ( 'NONE',  ( -1.073225997510925892E-13, 0.000000000000000000, -1.000000000000000000 ) ) ;
#15729 = EDGE_CURVE ( 'NONE', #7197, #18734, #17260, .T. ) ;
#15730 = ORIENTED_EDGE ( 'NONE', *, *, #20301, .T. ) ;
#15731 = CARTESIAN_POINT ( 'NONE',  ( 0.000000000000000000, -3695.699999999999818, 2239.009999999999764 ) ) ;
#15732 = CARTESIAN_POINT ( 'NONE',  ( 15.54478274857000031, -3659.509919104000346, 2250.166342301999521 ) ) ;
#15733 = LINE ( 'NONE', #17593, #15837 ) ;
#15734 = LOCAL_TIME ( 17, 37, 43.00000000000000000, #2907 ) ;
#15735 =( GEOMETRIC_REPRESENTATION_CONTEXT ( 3 ) GLOBAL_UNCERTAINTY_ASSIGNED_CONTEXT ( ( #5748 ) ) GLOBAL_UNIT_ASSIGNED_CONTEXT ( ( #9985, #8009, #6259 ) ) REPRESENTATION_CONTEXT ( 'NONE', 'WORKASPACE' ) );
#15736 = DIRECTION ( 'NONE',  ( 1.000000000000000000, 0.000000000000000000, 0.000000000000000000 ) ) ;
#15737 = EDGE_CURVE ( 'NONE', #22010, #1650, #10135, .T. ) ;
#15738 = CALENDAR_DATE ( 2026, 26, 10 ) ;
#15739 = EDGE_CURVE ( 'NONE', #10014, #15650, #22428, .T. ) ;
#15740 = CARTESIAN_POINT ( 'NONE',  ( 76.20000000000000284, -3568.700000000000273, 2259.837999999999738 ) ) ;
#15741 = DIRECTION ( 'NONE',  ( 0.000000000000000000, 0.000000000000000000, 1.000000000000000000 ) ) ;
#15742 = CARTESIAN_POINT ( 'NONE',  ( 11.34365660141000021, -3601.846755679000125, 2296.210799999999836 ) ) ;
#15743 = PRODUCT_DEFINITION_SHAPE ( 'NONE', 'NONE',  #9636 ) ;
#15744 = CARTESIAN_POINT ( 'NONE',  ( 141.8623322999648337, -3657.656292019905322, 2248.779374755923982 ) ) ;
#15745 = ORIENTED_EDGE ( 'NONE', *, *, #8824, .F. ) ;
#15746 = LINE ( 'NONE', #1556, #18211 ) ;
#15747 = EDGE_CURVE ( 'NONE', #16647, #825, #10024, .T. ) ;
#15748 = VERTEX_POINT ( 'NONE', #8269 ) ;
#15749 = ORIENTED_EDGE ( 'NONE', *, *, #5959, .F. ) ;
#15750 = APPROVAL_PERSON_ORGANIZATION ( #18716, #6053, #9704 ) ;
#15751 = APPROVAL_PERSON_ORGANIZATION ( #19455, #17344, #5170 ) ;
#15752 = ORIENTED_EDGE ( 'NONE', *, *, #5992, .F. ) ;
#15753 = AXIS2_PLACEMENT_3D ( 'NONE', #1160, #10069, #1050 ) ;
#15754 = CARTESIAN_POINT ( 'NONE',  ( 145.3795747169000094, -3578.859731361000286, 2244.547525601999951 ) ) ;
#15755 = ORIENTED_EDGE ( 'NONE', *, *, #22160, .T. ) ;
#15756 = ORIENTED_EDGE ( 'NONE', *, *, #18733, .F. ) ;
#15757 = DIRECTION ( 'NONE',  ( -1.052267375338999979E-13, 2.590196616219000170E-13, -1.000000000000000000 ) ) ;
#15758 = DIRECTION ( 'NONE',  ( 0.000000000000000000, 0.000000000000000000, -1.000000000000000000 ) ) ;
#15759 = DIRECTION ( 'NONE',  ( 0.000000000000000000, -1.000000000000000000, 0.000000000000000000 ) ) ;
#15760 = EDGE_LOOP ( 'NONE', ( #17061, #19326, #4845, #3314 ) ) ;
#15761 = CARTESIAN_POINT ( 'NONE',  ( 50.79999999999999716, -3619.500000000000000, 2259.837999999999738 ) ) ;
#15762 = DIRECTION ( 'NONE',  ( 0.000000000000000000, 0.000000000000000000, -1.000000000000000000 ) ) ;
#15763 = CARTESIAN_POINT ( 'NONE',  ( 25.39999999999999858, -3660.140000000000327, 2244.547199999999975 ) ) ;
#15764 = DIRECTION ( 'NONE',  ( 0.5000000000048030468, 0.8660254037816655925, 0.000000000000000000 ) ) ;
#15765 = VERTEX_POINT ( 'NONE', #4752 ) ;
#15766 = ADVANCED_FACE ( 'NONE', ( #11902 ), #19051, .T. ) ;
#15767 = CALENDAR_DATE ( 2026, 26, 10 ) ;
#15768 = EDGE_LOOP ( 'NONE', ( #23011, #22241, #8385, #18456, #19959, #9812 ) ) ;
#15769 = CARTESIAN_POINT ( 'NONE',  ( -5.588000000000000078, -3694.938000000000102, 2228.849999999999909 ) ) ;
#15770 = CARTESIAN_POINT ( 'NONE',  ( 10.45683289038945674, -3581.244648887170115, 2248.943261231277575 ) ) ;
#15771 = PERSON ( 'NAUO-PER6', 'UNSPECIFIED', 'UNSPECIFIED', ('UNSPECIFIED'), ('UNSPECIFIED'), ('UNSPECIFIED') ) ;
#15772 = EDGE_LOOP ( 'NONE', ( #10462, #14758, #625, #12136, #8674, #11365 ) ) ;
#15773 = VECTOR ( 'NONE', #11431, 1000.000000000000000 ) ;
#15774 = VERTEX_POINT ( 'NONE', #5460 ) ;
#15775 = PLANE ( 'NONE',  #3602 ) ;
#15776 = AXIS2_PLACEMENT_3D ( 'NONE', #20088, #1918, #2162 ) ;
#15777 = CYLINDRICAL_SURFACE ( 'NONE', #9890, 0.3809999999999303388 ) ;
#15778 = CARTESIAN_POINT ( 'NONE',  ( 145.1382046083306534, -3577.698739476651099, 2244.777305218250604 ) ) ;
#15779 = DIRECTION ( 'NONE',  ( -1.000000000000000000, 0.000000000000000000, 0.000000000000000000 ) ) ;
#15780 = CARTESIAN_POINT ( 'NONE',  ( 10.57261563002993832, -3661.393710553322762, 2249.945659169295141 ) ) ;
#15781 = APPLIED_PERSON_AND_ORGANIZATION_ASSIGNMENT ( #6976, #16103, ( #15394 ) ) ;
#15782 = CARTESIAN_POINT ( 'NONE',  ( 147.3681911278365533, -3544.023782195929925, 2260.479223148535311 ) ) ;
#15783 = ORIENTED_EDGE ( 'NONE', *, *, #1191, .T. ) ;
#15784 = CARTESIAN_POINT ( 'NONE',  ( 137.3683132029985927, -3578.148799999858966, 2239.391000000000076 ) ) ;
#15785 = CARTESIAN_POINT ( 'NONE',  ( 76.20000000000000284, -3568.700000000000273, 2239.771999999999935 ) ) ;
#15786 = FACE_OUTER_BOUND ( 'NONE', #2096, .T. ) ;
#15787 = CARTESIAN_POINT ( 'NONE',  ( 95.25000000000000000, -3694.430000000000291, 2247.392000000000280 ) ) ;
#15788 = FACE_OUTER_BOUND ( 'NONE', #18131, .T. ) ;
#15789 = AXIS2_PLACEMENT_3D ( 'NONE', #734, #22065, #20429 ) ;
#15790 = VERTEX_POINT ( 'NONE', #8856 ) ;
#15791 = VECTOR ( 'NONE', #4679, 1000.000000000000000 ) ;
#15792 = DIRECTION ( 'NONE',  ( -2.324635735433000053E-14, 2.336881798971000105E-14, -1.000000000000000000 ) ) ;
#15793 = B_SPLINE_CURVE_WITH_KNOTS ( 'NONE', 3,
 ( #16441, #2037, #21723, #5677 ),
 .UNSPECIFIED., .F., .F.,
 ( 4, 4 ),
 ( 0.000000000000000000, 1.000000000000000000 ),
 .UNSPECIFIED. ) ;
#15794 = VERTEX_POINT ( 'NONE', #14484 ) ;
#15795 = CARTESIAN_POINT ( 'NONE',  ( 9.698254030477786003, -3543.300000000000182, 2254.617539516272700 ) ) ;
#15796 = DIRECTION ( 'NONE',  ( 0.000000000000000000, 0.000000000000000000, -1.000000000000000000 ) ) ;
#15797 = CYLINDRICAL_SURFACE ( 'NONE', #21354, 5.715000000000997282 ) ;
#15798 = LINE ( 'NONE', #8420, #9573 ) ;
#15799 = FACE_OUTER_BOUND ( 'NONE', #11751, .T. ) ;
#15800 = CARTESIAN_POINT ( 'NONE',  ( 19.05000000000000071, -3663.315000000000509, 2247.392000000000280 ) ) ;
#15801 = AXIS2_PLACEMENT_3D ( 'NONE', #16310, #18408, #267 ) ;
#15802 = DIRECTION ( 'NONE',  ( 0.000000000000000000, 0.000000000000000000, 1.000000000000000000 ) ) ;
#15803 = ORIENTED_EDGE ( 'NONE', *, *, #16262, .T. ) ;
#15804 = CIRCLE ( 'NONE', #12443, 2.844799999999999773 ) ;
#15805 = DIRECTION ( 'NONE',  ( 0.000000000000000000, 0.000000000000000000, -1.000000000000000000 ) ) ;
#15806 = APPLIED_PERSON_AND_ORGANIZATION_ASSIGNMENT ( #5107, #13536, ( #10501 ) ) ;
#15807 = CARTESIAN_POINT ( 'NONE',  ( 12.69999999999999929, -3579.494999999999891, 2244.978999999999814 ) ) ;
#15808 = VERTEX_POINT ( 'NONE', #14133 ) ;
#15809 = FACE_OUTER_BOUND ( 'NONE', #14760, .T. ) ;
#15810 = ADVANCED_FACE ( 'NONE', ( #9202 ), #16115, .F. ) ;
#15811 = EDGE_LOOP ( 'NONE', ( #22245, #806 ) ) ;
#15812 = LINE ( 'NONE', #22598, #10175 ) ;
#15813 = ADVANCED_FACE ( 'NONE', ( #7330 ), #12363, .T. ) ;
#15814 = AXIS2_PLACEMENT_3D ( 'NONE', #21828, #11165, #2376 ) ;
#15815 = EDGE_LOOP ( 'NONE', ( #7209, #6633 ) ) ;
#15816 = VERTEX_POINT ( 'NONE', #9084 ) ;
#15817 = EDGE_CURVE ( 'NONE', #14376, #4689, #11285, .T. ) ;
#15818 = CARTESIAN_POINT ( 'NONE',  ( 137.3683132029000262, -3660.851200000000063, 2242.820000000000164 ) ) ;
#15819 = DATE_AND_TIME ( #9114, #5656 ) ;
#15820 = VERTEX_POINT ( 'NONE', #12714 ) ;
#15822 = CARTESIAN_POINT ( 'NONE',  ( 131.8608747668832564, -3695.477144326939651, 2260.051190193429193 ) ) ;
#15821 = VECTOR ( 'NONE', #5104, 1000.000000000000227 ) ;
#15823 = PERSON_AND_ORGANIZATION_ROLE ( 'design_supplier' ) ;
#15824 = AXIS2_PLACEMENT_3D ( 'NONE', #5068, #10334, #7067 ) ;
#15825 = CARTESIAN_POINT ( 'NONE',  ( 136.6529205195000145, -3695.699999999999818, 2254.503999999999905 ) ) ;
#15826 = EDGE_CURVE ( 'NONE', #3143, #7313, #14909, .T. ) ;
#15827 = CARTESIAN_POINT ( 'NONE',  ( 15.27563337016521317, -3580.706179722078105, 2249.559177238421853 ) ) ;
#15828 = CARTESIAN_POINT ( 'NONE',  ( 12.69999999999999929, -3659.504999999999654, 2272.030000000000200 ) ) ;
#15829 = LINE ( 'NONE', #19459, #3481 ) ;
#15830 = EDGE_CURVE ( 'NONE', #14734, #523, #19628, .T. ) ;
#15831 = CARTESIAN_POINT ( 'NONE',  ( 116.8400000000000034, -3544.570000000000164, 2247.392000000000280 ) ) ;
#15832 = VERTEX_POINT ( 'NONE', #177 ) ;
#15833 = AXIS2_PLACEMENT_3D ( 'NONE', #6098, #19926, #8426 ) ;
#15834 = CARTESIAN_POINT ( 'NONE',  ( 151.1299999999999955, -3544.570000000000164, 2259.329999999999927 ) ) ;
#15835 = FACE_OUTER_BOUND ( 'NONE', #3020, .T. ) ;
#15836 = ORIENTED_EDGE ( 'NONE', *, *, #5931, .T. ) ;
#15837 = VECTOR ( 'NONE', #4716, 1000.000000000000000 ) ;
#15838 = AXIS2_PLACEMENT_3D ( 'NONE', #5057, #10442, #10087 ) ;
#15839 = DIRECTION ( 'NONE',  ( 0.000000000000000000, 0.000000000000000000, -1.000000000000000000 ) ) ;
#15840 = ORIENTED_EDGE ( 'NONE', *, *, #3061, .T. ) ;
#15841 = ORIENTED_EDGE ( 'NONE', *, *, #13275, .F. ) ;
#15842 = EDGE_LOOP ( 'NONE', ( #2241, #6179, #17843, #12931 ) ) ;
#15843 = PLANE ( 'NONE',  #3790 ) ;
#15844 = DIRECTION ( 'NONE',  ( -1.000000000000000000, 0.000000000000000000, 0.000000000000000000 ) ) ;
#15845 = VERTEX_POINT ( 'NONE', #10952 ) ;
#15846 = EDGE_CURVE ( 'NONE', #22551, #3991, #20716, .T. ) ;
#15847 = CARTESIAN_POINT ( 'NONE',  ( 139.6999999999999886, -3579.494999999999891, 2245.359999999999673 ) ) ;
#15848 = CARTESIAN_POINT ( 'NONE',  ( 15.48106116729000092, -3600.123614707999877, 2279.464089926999804 ) ) ;
#15849 = CARTESIAN_POINT ( 'NONE',  ( 136.8603346907000002, -3579.284436177999851, 2250.207695148999846 ) ) ;
#15850 = AXIS2_PLACEMENT_3D ( 'NONE', #14310, #14076, #20990 ) ;
#15851 = PERSON_AND_ORGANIZATION ( #5446, #1895 ) ;
#15852 = EDGE_CURVE ( 'NONE', #20464, #4732, #6442, .T. ) ;
#15853 = ADVANCED_FACE ( 'NONE', ( #6991 ), #21390, .T. ) ;
#15854 = CARTESIAN_POINT ( 'NONE',  ( 28.24479999999899604, -3670.300000000000182, 2259.837999999999738 ) ) ;
#15855 = CARTESIAN_POINT ( 'NONE',  ( 9.989282597016131859, -3695.380630527866288, 2255.346357850532968 ) ) ;
#15856 = DIRECTION ( 'NONE',  ( 2.902585187577999742E-13, 4.457650181899999573E-12, -1.000000000000000000 ) ) ;
#15857 = AXIS2_PLACEMENT_3D ( 'NONE', #569, #22009, #13108 ) ;
#15858 = VECTOR ( 'NONE', #364, 1000.000000000000000 ) ;
#15859 = DIRECTION ( 'NONE',  ( -1.000000000000000000, 0.000000000000000000, 0.000000000000000000 ) ) ;
#15860 = ORIENTED_EDGE ( 'NONE', *, *, #21726, .T. ) ;
#15861 = DIRECTION ( 'NONE',  ( 6.119339505807659940E-14, -1.000000000000000000, 0.000000000000000000 ) ) ;
#15862 = ORIENTED_EDGE ( 'NONE', *, *, #16934, .T. ) ;
#15863 = EDGE_LOOP ( 'NONE', ( #18361, #4218, #8617, #4362 ) ) ;
#15864 = ORIENTED_EDGE ( 'NONE', *, *, #20139, .F. ) ;
#15865 = AXIS2_PLACEMENT_3D ( 'NONE', #3957, #20137, #10992 ) ;
#15866 = EDGE_CURVE ( 'NONE', #15808, #13348, #19910, .T. ) ;
#15867 = DIRECTION ( 'NONE',  ( 0.000000000000000000, 1.000000000000000000, 0.000000000000000000 ) ) ;
#15868 = ORIENTED_EDGE ( 'NONE', *, *, #7941, .T. ) ;
#15869 = ORIENTED_EDGE ( 'NONE', *, *, #16255, .T. ) ;
#15870 = FACE_OUTER_BOUND ( 'NONE', #12345, .T. ) ;
#15871 = APPROVAL_DATE_TIME ( #1684, #20937 ) ;
#15872 = DIRECTION ( 'NONE',  ( 1.000000000000000000, 1.224646799147353207E-16, 0.000000000000000000 ) ) ;
#15873 = DIRECTION ( 'NONE',  ( 6.341789985291834412E-14, 0.000000000000000000, 1.000000000000000000 ) ) ;
#15874 = VERTEX_POINT ( 'NONE', #20322 ) ;
#15875 = CARTESIAN_POINT ( 'NONE',  ( 137.1599999999999966, -3580.776127254000130, 2255.774000000000342 ) ) ;
#15876 = CARTESIAN_POINT ( 'NONE',  ( 57.14999999999999858, -3694.430000000000291, 2247.392000000000280 ) ) ;
#15877 = CYLINDRICAL_SURFACE ( 'NONE', #6847, 2.844800000000091700 ) ;
#15878 = CARTESIAN_POINT ( 'NONE',  ( 127.0000000000000000, -3660.140000000000327, 2247.392000000000280 ) ) ;
#15879 = VERTEX_POINT ( 'NONE', #4150 ) ;
#15880 = COORDINATED_UNIVERSAL_TIME_OFFSET ( 0, 0, .AHEAD. ) ;
#15881 = ADVANCED_FACE ( 'NONE', ( #13058 ), #18665, .F. ) ;
#15882 = ADVANCED_FACE ( 'NONE', ( #7897 ), #14932, .T. ) ;
#15883 = VERTEX_POINT ( 'NONE', #14823 ) ;
#15884 = DIRECTION ( 'NONE',  ( -1.000000000000000000, 0.000000000000000000, 0.000000000000000000 ) ) ;
#15885 = EDGE_CURVE ( 'NONE', #13759, #20359, #4549, .T. ) ;
#15886 = AXIS2_PLACEMENT_3D ( 'NONE', #14022, #19407, #5232 ) ;
#15887 = CARTESIAN_POINT ( 'NONE',  ( 10.27313954880075109, -3580.979417148001176, 2249.290044219352239 ) ) ;
#15888 = VERTEX_POINT ( 'NONE', #8015 ) ;
#15889 = FACE_OUTER_BOUND ( 'NONE', #18648, .T. ) ;
#15890 = AXIS2_PLACEMENT_3D ( 'NONE', #6889, #17765, #21060 ) ;
#15891 = ADVANCED_FACE ( 'NONE', ( #4265 ), #2509, .T. ) ;
#15892 = VERTEX_POINT ( 'NONE', #13276 ) ;
#15893 = DIRECTION ( 'NONE',  ( 0.000000000000000000, 0.000000000000000000, 1.000000000000000000 ) ) ;
#15894 = DIRECTION ( 'NONE',  ( 0.000000000000000000, -1.000000000000000000, 0.000000000000000000 ) ) ;
#15895 = PLANE ( 'NONE',  #2853 ) ;
#15896 = EDGE_CURVE ( 'NONE', #22386, #204, #4485, .T. ) ;
#15897 = CARTESIAN_POINT ( 'NONE',  ( 11.22865419974734102, -3661.939788859982855, 2249.595128560251851 ) ) ;
#15898 = EDGE_CURVE ( 'NONE', #3611, #21098, #19145, .T. ) ;
#15899 = CARTESIAN_POINT ( 'NONE',  ( 0.7620000000000000107, -3694.938000000000102, 2296.591799999999694 ) ) ;
#15900 = VERTEX_POINT ( 'NONE', #6265 ) ;
#15901 = DIRECTION ( 'NONE',  ( 0.000000000000000000, 1.000000000000000000, 0.000000000000000000 ) ) ;
#15902 = AXIS2_PLACEMENT_3D ( 'NONE', #12200, #21456, #10439 ) ;
#15903 = DIRECTION ( 'NONE',  ( 0.000000000000000000, 0.000000000000000000, -1.000000000000000000 ) ) ;
#15904 = AXIS2_PLACEMENT_3D ( 'NONE', #7058, #4842, #13638 ) ;
#15905 = DIRECTION ( 'NONE',  ( 0.000000000000000000, 0.000000000000000000, 1.000000000000000000 ) ) ;
#15906 = CIRCLE ( 'NONE', #22236, 5.460999999999938126 ) ;
#15907 = CARTESIAN_POINT ( 'NONE',  ( 14.94580037973010889, -3657.758775493699432, 2248.948511419066108 ) ) ;
#15908 = DIRECTION ( 'NONE',  ( 1.000000000000000000, 0.000000000000000000, 0.000000000000000000 ) ) ;
#15909 = VERTEX_POINT ( 'NONE', #20208 ) ;
#15910 = DIRECTION ( 'NONE',  ( 0.000000000000000000, 0.000000000000000000, 1.000000000000000000 ) ) ;
#15911 = ORIENTED_EDGE ( 'NONE', *, *, #19227, .T. ) ;
#15912 = CARTESIAN_POINT ( 'NONE',  ( 3.810000000000000053, -3543.299999999999727, 2228.849999999999909 ) ) ;
#15913 = LINE ( 'NONE', #19893, #13761 ) ;
#15914 = CALENDAR_DATE ( 2026, 26, 10 ) ;
#15915 = DIRECTION ( 'NONE',  ( 0.000000000000000000, 0.000000000000000000, -1.000000000000000000 ) ) ;
#15916 = CARTESIAN_POINT ( 'NONE',  ( 61.26424768829000556, -3544.061999999999898, 2279.065800000000309 ) ) ;
#15917 = LINE ( 'NONE', #3485, #14080 ) ;
#15918 = AXIS2_PLACEMENT_3D ( 'NONE', #1067, #19121, #10090 ) ;
#15919 = CIRCLE ( 'NONE', #21525, 0.7619999999999987894 ) ;
#15920 = LINE ( 'NONE', #14169, #18607 ) ;
#15921 = VECTOR ( 'NONE', #10061, 1000.000000000000000 ) ;
#15922 = FACE_BOUND ( 'NONE', #8266, .T. ) ;
#15923 = VECTOR ( 'NONE', #22856, 1000.000000000000000 ) ;
#15924 = CARTESIAN_POINT ( 'NONE',  ( 0.7620000000000000107, -3543.299999999999727, 2295.829799999999977 ) ) ;
#15925 = EDGE_LOOP ( 'NONE', ( #380, #12782, #1374, #15356, #1618, #6280, #18086, #9413 ) ) ;
#15926 = DIRECTION ( 'NONE',  ( 0.000000000000000000, 0.8660254037820785955, -0.5000000000040877302 ) ) ;
#15927 = FACE_OUTER_BOUND ( 'NONE', #17449, .T. ) ;
#15928 = VERTEX_POINT ( 'NONE', #18441 ) ;
#15929 = DIRECTION ( 'NONE',  ( 1.000000000000000000, 0.000000000000000000, 0.000000000000000000 ) ) ;
#15930 = ORIENTED_EDGE ( 'NONE', *, *, #5407, .T. ) ;
#15931 = CARTESIAN_POINT ( 'NONE',  ( 127.0000000000000000, -3578.860000000000127, 2244.547199999999975 ) ) ;
#15932 = AXIS2_PLACEMENT_3D ( 'NONE', #6890, #3354, #12382 ) ;
#15933 = EDGE_LOOP ( 'NONE', ( #1506, #13584, #16854, #470, #14982 ) ) ;
#15934 = CIRCLE ( 'NONE', #17038, 3.175000000000149925 ) ;
#15935 = CARTESIAN_POINT ( 'NONE',  ( 55.57575231171000496, -3694.938000000000102, 2275.763800000000174 ) ) ;
#15936 = ORIENTED_EDGE ( 'NONE', *, *, #4484, .F. ) ;
#15937 =( BOUNDED_CURVE ( )  B_SPLINE_CURVE ( 3, ( #3242, #10389, #19529, #3468 ),
 .UNSPECIFIED., .F., .T. ) 
 B_SPLINE_CURVE_WITH_KNOTS ( ( 4, 4 ),
 ( 1.570796326807037513, 3.141592653589829975 ),
 .UNSPECIFIED. ) 
 CURVE ( )  GEOMETRIC_REPRESENTATION_ITEM ( )  RATIONAL_B_SPLINE_CURVE ( ( 1.000000000000000000, 0.8047378541272178776, 0.8047378541272178776, 1.000000000000000000 ) ) 
 REPRESENTATION_ITEM ( '' )  );
#15938 = DATE_AND_TIME ( #18041, #1893 ) ;
#15939 = APPLIED_PERSON_AND_ORGANIZATION_ASSIGNMENT ( #16789, #16449, ( #22059 ) ) ;
#15940 = DIRECTION ( 'NONE',  ( 0.000000000000000000, 0.000000000000000000, 1.000000000000000000 ) ) ;
#15941 = VECTOR ( 'NONE', #10452, 1000.000000000000114 ) ;
#15942 = CARTESIAN_POINT ( 'NONE',  ( 15.35573774336631914, -3580.514832482311249, 2249.705997884422686 ) ) ;
#15943 = DIRECTION ( 'NONE',  ( 0.000000000000000000, 1.000000000000000000, 0.000000000000000000 ) ) ;
#15944 = CARTESIAN_POINT ( 'NONE',  ( 9.916854418464000176, -3578.905956564000007, 2250.236428761999832 ) ) ;
#15945 = ADVANCED_FACE ( 'NONE', ( #2396 ), #13398, .F. ) ;
#15946 = ADVANCED_FACE ( 'NONE', ( #20532 ), #18555, .F. ) ;
#15947 = DIRECTION ( 'NONE',  ( 0.000000000000000000, 0.000000000000000000, 1.000000000000000000 ) ) ;
#15948 = EDGE_LOOP ( 'NONE', ( #19801, #12042, #1345, #14680 ) ) ;
#15949 = AXIS2_PLACEMENT_3D ( 'NONE', #22215, #18598, #4765 ) ;
#15950 = CARTESIAN_POINT ( 'NONE',  ( 15.41076828073257055, -3695.380630529619793, 2255.346378162581459 ) ) ;
#15951 = EDGE_CURVE ( 'NONE', #17917, #7027, #22131, .T. ) ;
#15952 = VECTOR ( 'NONE', #18018, 1000.000000000000000 ) ;
#15953 = DIRECTION ( 'NONE',  ( -0.8660254037840939834, -0.5000000000005969669, 0.000000000000000000 ) ) ;
#15954 = ORIENTED_EDGE ( 'NONE', *, *, #2265, .T. ) ;
#15955 = AXIS2_PLACEMENT_3D ( 'NONE', #13663, #4758, #17169 ) ;
#15956 = CARTESIAN_POINT ( 'NONE',  ( 12.69999999999999929, -3599.497499999999945, 2290.622800000000097 ) ) ;
#15957 = CIRCLE ( 'NONE', #2525, 2.844799999999961582 ) ;
#15958 = ORIENTED_EDGE ( 'NONE', *, *, #10451, .T. ) ;
#15959 = EDGE_CURVE ( 'NONE', #9431, #9191, #16450, .T. ) ;
#15960 = TOROIDAL_SURFACE ( 'NONE', #14848, 3.606799999999999784, 0.7620000000000000107 ) ;
#15961 = CARTESIAN_POINT ( 'NONE',  ( 145.1609999999999729, -3579.494999999999891, 2244.978999999999814 ) ) ;
#15962 = CARTESIAN_POINT ( 'NONE',  ( 20.32000000000000028, -3544.061999999999898, 2289.213099999999940 ) ) ;
#15963 = ORIENTED_EDGE ( 'NONE', *, *, #2768, .T. ) ;
#15964 = CARTESIAN_POINT ( 'NONE',  ( 20.32000000000000028, -3658.235000000000127, 2247.392000000000280 ) ) ;
#15965 = DIRECTION ( 'NONE',  ( 0.000000000000000000, 1.000000000000000000, 0.000000000000000000 ) ) ;
#15966 = APPLICATION_PROTOCOL_DEFINITION ( 'international standard', 'automotive_design', 2000, #1255 ) ;
#15967 = AXIS2_PLACEMENT_3D ( 'NONE', #4032, #19622, #11057 ) ;
#15968 = CARTESIAN_POINT ( 'NONE',  ( 15.54479999999999862, -3639.502500000000055, 2288.971800000000258 ) ) ;
#15969 = CARTESIAN_POINT ( 'NONE',  ( 117.9067999999989951, -3594.099999999999909, 2239.009999999999764 ) ) ;
#15970 = TOROIDAL_SURFACE ( 'NONE', #12614, 3.606799999999999784, 0.7620000000000000107 ) ;
#15971 = VECTOR ( 'NONE', #9763, 1000.000000000000000 ) ;
#15972 = CARTESIAN_POINT ( 'NONE',  ( 137.9080942012932951, -3657.295453499272298, 2247.303175097353687 ) ) ;
#15973 = EDGE_CURVE ( 'NONE', #4104, #15991, #520, .T. ) ;
#15974 = ADVANCED_FACE ( 'NONE', ( #5807 ), #18030, .T. ) ;
#15975 = VERTEX_POINT ( 'NONE', #20098 ) ;
#15976 = ADVANCED_FACE ( 'NONE', ( #16567 ), #16679, .T. ) ;
#15977 = CARTESIAN_POINT ( 'NONE',  ( 137.1196777603386181, -3660.705328851377089, 2250.180928057881374 ) ) ;
#15978 = EDGE_CURVE ( 'NONE', #16093, #20661, #22519, .T. ) ;
#15979 = ORIENTED_EDGE ( 'NONE', *, *, #19451, .T. ) ;
#15980 = ORIENTED_EDGE ( 'NONE', *, *, #5229, .T. ) ;
#15981 = ORIENTED_EDGE ( 'NONE', *, *, #20739, .T. ) ;
#15982 = AXIS2_PLACEMENT_3D ( 'NONE', #12193, #1636, #19344 ) ;
#15983 = AXIS2_PLACEMENT_3D ( 'NONE', #6612, #12331, #19481 ) ;
#15984 = CARTESIAN_POINT ( 'NONE',  ( 7.238999999999998991, -3659.504999999999654, 2244.978999999999814 ) ) ;
#15985 = ORIENTED_EDGE ( 'NONE', *, *, #5665, .F. ) ;
#15986 = EDGE_LOOP ( 'NONE', ( #20064, #19332, #14244, #2134 ) ) ;
#15987 = CARTESIAN_POINT ( 'NONE',  ( 151.4000000000000057, -3695.699999999999818, 2239.039032635400417 ) ) ;
#15988 = APPROVAL_DATE_TIME ( #17972, #14062 ) ;
#15989 = CARTESIAN_POINT ( 'NONE',  ( 101.5999999999999943, -3619.500000000000000, 2261.869999999999891 ) ) ;
#15990 = CARTESIAN_POINT ( 'NONE',  ( 127.0000000000000000, -3619.500000000000000, 2239.009999999999764 ) ) ;
#15991 = VERTEX_POINT ( 'NONE', #6616 ) ;
#15992 = CARTESIAN_POINT ( 'NONE',  ( 97.99320000000000164, -3619.500000000000000, 2260.600000000000364 ) ) ;
#15993 = CARTESIAN_POINT ( 'NONE',  ( 57.14999999999999858, -3568.700000000000273, 2247.392000000000280 ) ) ;
#15994 = DIRECTION ( 'NONE',  ( 0.000000000000000000, 0.000000000000000000, 1.000000000000000000 ) ) ;
#15995 = EDGE_CURVE ( 'NONE', #7858, #4050, #22635, .T. ) ;
#15996 = CARTESIAN_POINT ( 'NONE',  ( 114.2999999999999972, -3594.099999999999909, 2239.771999999999935 ) ) ;
#15997 = VERTEX_POINT ( 'NONE', #10224 ) ;
#15998 = PERSON_AND_ORGANIZATION ( #5446, #1895 ) ;
#15999 = EDGE_LOOP ( 'NONE', ( #20378, #14036, #11056, #16412, #1087 ) ) ;
#16000 = CARTESIAN_POINT ( 'NONE',  ( 131.7408816625886345, -3543.371700234166838, 2259.750712803343049 ) ) ;
#16001 = DIRECTION ( 'NONE',  ( 1.000000000000000000, 0.000000000000000000, 0.000000000000000000 ) ) ;
#16002 = CIRCLE ( 'NONE', #22713, 4.114799999999974034 ) ;
#16003 = DIRECTION ( 'NONE',  ( 0.000000000000000000, 0.000000000000000000, -1.000000000000000000 ) ) ;
#16004 = EDGE_CURVE ( 'NONE', #20079, #21067, #1561, .T. ) ;
#16005 = EDGE_LOOP ( 'NONE', ( #15493, #12278, #21429, #12391, #20334, #12584 ) ) ;
#16006 = DIRECTION ( 'NONE',  ( 2.330758767201999921E-14, 1.000000000000000000, 0.000000000000000000 ) ) ;
#16007 = DIRECTION ( 'NONE',  ( 1.000000000000000000, 0.000000000000000000, 0.000000000000000000 ) ) ;
#16008 = CARTESIAN_POINT ( 'NONE',  ( 144.5184724295484671, -3576.421590092805673, 2245.925647645899062 ) ) ;
#16009 = FACE_OUTER_BOUND ( 'NONE', #3594, .T. ) ;
#16010 = DIRECTION ( 'NONE',  ( 0.000000000000000000, 0.000000000000000000, 1.000000000000000000 ) ) ;
#16011 = EDGE_CURVE ( 'NONE', #6769, #16761, #14673, .T. ) ;
#16012 = EDGE_CURVE ( 'NONE', #21114, #11744, #7555, .T. ) ;
#16013 = FACE_OUTER_BOUND ( 'NONE', #4583, .T. ) ;
#16014 = ORIENTED_EDGE ( 'NONE', *, *, #22429, .T. ) ;
#16015 = EDGE_CURVE ( 'NONE', #20116, #6254, #449, .T. ) ;
#16016 = CARTESIAN_POINT ( 'NONE',  ( 3.048000000000000043, -3694.938000000000102, 2228.849999999999909 ) ) ;
#16017 = CARTESIAN_POINT ( 'NONE',  ( -12.69999999999999929, -3660.140000000000327, 2247.392000000000280 ) ) ;
#16018 = AXIS2_PLACEMENT_3D ( 'NONE', #3016, #15679, #6780 ) ;
#16019 = DIRECTION ( 'NONE',  ( 0.000000000000000000, -1.000000000000000000, 0.000000000000000000 ) ) ;
#16020 = CARTESIAN_POINT ( 'NONE',  ( 15.35765731516040056, -3658.489959486714270, 2249.709633093460980 ) ) ;
#16021 = CARTESIAN_POINT ( 'NONE',  ( 136.8825577675800105, -3695.562642952237638, 2255.079235783421609 ) ) ;
#16022 = ORIENTED_EDGE ( 'NONE', *, *, #23003, .F. ) ;
#16023 = EDGE_CURVE ( 'NONE', #22010, #10134, #13540, .T. ) ;
#16024 = CARTESIAN_POINT ( 'NONE',  ( 1.270000000000000018, -3578.860000000000127, 2243.277199999999993 ) ) ;
#16025 = VERTEX_POINT ( 'NONE', #21016 ) ;
#16026 = VECTOR ( 'NONE', #10551, 1000.000000000000000 ) ;
#16027 = FACE_OUTER_BOUND ( 'NONE', #16106, .T. ) ;
#16028 = CARTESIAN_POINT ( 'NONE',  ( 10.01184914621919653, -3543.672816122378208, 2255.402917874179821 ) ) ;
#16029 = COORDINATED_UNIVERSAL_TIME_OFFSET ( 0, 0, .AHEAD. ) ;
#16030 = EDGE_CURVE ( 'NONE', #18590, #22471, #2722, .T. ) ;
#16031 = CARTESIAN_POINT ( 'NONE',  ( 12.69999999999999929, -3648.710000000000036, 2257.592639999999847 ) ) ;
#16032 = ADVANCED_FACE ( 'NONE', ( #8362 ), #10105, .T. ) ;
#16033 = DIRECTION ( 'NONE',  ( 0.000000000000000000, 0.000000000000000000, -1.000000000000000000 ) ) ;
#16034 = CARTESIAN_POINT ( 'NONE',  ( 14.61266695128000137, -3657.399152860999493, 2246.630000000000109 ) ) ;
#16035 = LINE ( 'NONE', #17904, #11475 ) ;
#16036 = AXIS2_PLACEMENT_3D ( 'NONE', #1436, #19486, #21364 ) ;
#16037 = ORIENTED_EDGE ( 'NONE', *, *, #22015, .F. ) ;
#16038 = DIRECTION ( 'NONE',  ( -1.073225997510925892E-13, 0.000000000000000000, -1.000000000000000000 ) ) ;
#16039 = ORIENTED_EDGE ( 'NONE', *, *, #9239, .F. ) ;
#16040 = CARTESIAN_POINT ( 'NONE',  ( 10.36831320286361979, -3580.841200000155368, 2239.167815367206913 ) ) ;
#16041 = ADVANCED_FACE ( 'NONE', ( #22866 ), #15276, .F. ) ;
#16042 = CARTESIAN_POINT ( 'NONE',  ( 12.69999999999999929, -3639.502500000000055, 2296.591799999999694 ) ) ;
#16043 = ORIENTED_EDGE ( 'NONE', *, *, #14098, .F. ) ;
#16044 = CARTESIAN_POINT ( 'NONE',  ( 1.270000000000000018, -3578.860000000000127, 2250.236800000000130 ) ) ;
#16045 = EDGE_LOOP ( 'NONE', ( #21093, #4981 ) ) ;
#16046 = DIRECTION ( 'NONE',  ( 0.000000000000000000, 0.000000000000000000, 1.000000000000000000 ) ) ;
#16047 = CYLINDRICAL_SURFACE ( 'NONE', #7558, 2.844799999999999773 ) ;
#16048 = VERTEX_POINT ( 'NONE', #6842 ) ;
#16049 = ORIENTED_EDGE ( 'NONE', *, *, #17820, .F. ) ;
#16050 = CARTESIAN_POINT ( 'NONE',  ( 137.0385493787570965, -3580.499829900386885, 2249.716652619521483 ) ) ;
#16051 = ORIENTED_EDGE ( 'NONE', *, *, #2078, .F. ) ;
#16052 = VECTOR ( 'NONE', #12876, 1000.000000000000000 ) ;
#16053 = CARTESIAN_POINT ( 'NONE',  ( 60.65520000000000067, -3644.899999999999636, 2259.837999999999738 ) ) ;
#16054 = COORDINATED_UNIVERSAL_TIME_OFFSET ( 0, 0, .AHEAD. ) ;
#16055 = DIRECTION ( 'NONE',  ( -0.000000000000000000, -1.000000000000000000, -0.000000000000000000 ) ) ;
#16056 = DIRECTION ( 'NONE',  ( 0.000000000000000000, 0.000000000000000000, -1.000000000000000000 ) ) ;
#16057 = DIRECTION ( 'NONE',  ( 1.224646799141920914E-16, -1.000000000000000000, -2.336881798971000421E-14 ) ) ;
#16058 = DIRECTION ( 'NONE',  ( 1.000000000000000000, 0.000000000000000000, 0.000000000000000000 ) ) ;
#16059 = LINE ( 'NONE', #6817, #22204 ) ;
#16060 = ORIENTED_EDGE ( 'NONE', *, *, #3478, .F. ) ;
#16061 = CARTESIAN_POINT ( 'NONE',  ( 0.7620000000000000107, -3694.938000000000102, 2275.763800000000174 ) ) ;
#16062 = CARTESIAN_POINT ( 'NONE',  ( 14.90546723228000126, -3577.690681480999956, 2257.813182709000102 ) ) ;
#16063 = VERTEX_POINT ( 'NONE', #13755 ) ;
#16064 = CARTESIAN_POINT ( 'NONE',  ( 4.934178814895267884, -3695.321318630448332, 2260.234746714515040 ) ) ;
#16065 = AXIS2_PLACEMENT_3D ( 'NONE', #8875, #16019, #7116 ) ;
#16066 = DIRECTION ( 'NONE',  ( 0.000000000000000000, 0.000000000000000000, -1.000000000000000000 ) ) ;
#16067 = APPLIED_PERSON_AND_ORGANIZATION_ASSIGNMENT ( #10428, #8677, ( #8248 ) ) ;
#16068 = CARTESIAN_POINT ( 'NONE',  ( 20.34169023495000062, -3544.202533098000458, 2260.545675974999995 ) ) ;
#16069 = EDGE_LOOP ( 'NONE', ( #13245, #12861, #9546, #12201 ) ) ;
#16070 = CARTESIAN_POINT ( 'NONE',  ( 12.69999999994000106, -3596.365159094999854, 2296.591799999999694 ) ) ;
#16071 = CYLINDRICAL_SURFACE ( 'NONE', #9911, 3.175000000000149925 ) ;
#16072 = ORIENTED_EDGE ( 'NONE', *, *, #14607, .T. ) ;
#16073 = DIRECTION ( 'NONE',  ( 3.005032793049999585E-13, -2.590196616230999943E-13, -1.000000000000000000 ) ) ;
#16074 = CYLINDRICAL_SURFACE ( 'NONE', #20589, 1.269999999999900320 ) ;
#16075 = EDGE_CURVE ( 'NONE', #17394, #10503, #15387, .T. ) ;
#16076 =( LENGTH_UNIT ( ) NAMED_UNIT ( * ) SI_UNIT ( .MILLI., .METRE. ) );
#16077 = DIRECTION ( 'NONE',  ( 0.5000000000007065459, 0.8660254037840305896, 0.000000000000000000 ) ) ;
#16078 = PLANE ( 'NONE',  #9625 ) ;
#16079 = APPROVAL_ROLE ( '' ) ;
#16080 = ORIENTED_EDGE ( 'NONE', *, *, #12108, .F. ) ;
#16081 = AXIS2_PLACEMENT_3D ( 'NONE', #14016, #1584, #5228 ) ;
#16082 = EDGE_CURVE ( 'NONE', #565, #1438, #15418, .T. ) ;
#16083 = CARTESIAN_POINT ( 'NONE',  ( 35.56000000000000227, -3695.699999999999818, 2247.392000000000280 ) ) ;
#16084 = VERTEX_POINT ( 'NONE', #20646 ) ;
#16085 = PRODUCT_DEFINITION_FORMATION_WITH_SPECIFIED_SOURCE ( 'ANY', '', #6959, .NOT_KNOWN. ) ;
#16086 = CYLINDRICAL_SURFACE ( 'NONE', #19345, 2.844799999999009010 ) ;
#16087 = AXIS2_PLACEMENT_3D ( 'NONE', #6635, #17377, #1338 ) ;
#16088 = CARTESIAN_POINT ( 'NONE',  ( 137.0620653827227500, -3658.440016311159980, 2249.673027215405909 ) ) ;
#16089 = ORIENTED_EDGE ( 'NONE', *, *, #12746, .T. ) ;
#16090 = EDGE_LOOP ( 'NONE', ( #714, #9865 ) ) ;
#16091 = VERTEX_POINT ( 'NONE', #5075 ) ;
#16092 = DIRECTION ( 'NONE',  ( 0.000000000000000000, 0.000000000000000000, 1.000000000000000000 ) ) ;
#16093 = VERTEX_POINT ( 'NONE', #18896 ) ;
#16094 = ORIENTED_EDGE ( 'NONE', *, *, #1080, .F. ) ;
#16095 = ORIENTED_EDGE ( 'NONE', *, *, #20166, .F. ) ;
#16096 = AXIS2_PLACEMENT_3D ( 'NONE', #6675, #15448, #4785 ) ;
#16097 = APPROVAL ( #1514, 'UNSPECIFIED' ) ;
#16098 = DIRECTION ( 'NONE',  ( 1.224646799141920914E-16, -1.000000000000000000, -2.336881798971000421E-14 ) ) ;
#16099 = EDGE_LOOP ( 'NONE', ( #13998, #5558, #11189, #1391 ) ) ;
#16100 = EDGE_LOOP ( 'NONE', ( #9406, #19855, #15269, #7674 ) ) ;
#16101 = LOCAL_TIME ( 17, 37, 43.00000000000000000, #18412 ) ;
#16102 = DIRECTION ( 'NONE',  ( 0.000000000000000000, -0.8660254037840939834, -0.5000000000005969669 ) ) ;
#16103 = PERSON_AND_ORGANIZATION_ROLE ( 'classification_officer' ) ;
#16104 = DIRECTION ( 'NONE',  ( -0.9296367896487196525, 0.3684771897032736443, 0.000000000000000000 ) ) ;
#16105 = CARTESIAN_POINT ( 'NONE',  ( 142.4126867973298545, -3657.938829547075329, 2239.009999999999764 ) ) ;
#16106 = EDGE_LOOP ( 'NONE', ( #4366, #22224, #9771, #15509 ) ) ;
#16107 = DIRECTION ( 'NONE',  ( 0.000000000000000000, 1.000000000000000000, 0.000000000000000000 ) ) ;
#16108 = ADVANCED_FACE ( 'NONE', ( #1435 ), #13916, .T. ) ;
#16109 = FACE_BOUND ( 'NONE', #3065, .T. ) ;
#16110 = CARTESIAN_POINT ( 'NONE',  ( 6.985000002048998624, -3579.713624101183086, 2244.668992692460506 ) ) ;
#16111 = EDGE_CURVE ( 'NONE', #21367, #6441, #7193, .T. ) ;
#16112 = CARTESIAN_POINT ( 'NONE',  ( 20.32000000000000028, -3694.938000000000102, 2286.368300000000090 ) ) ;
#16113 = COORDINATED_UNIVERSAL_TIME_OFFSET ( 0, 0, .AHEAD. ) ;
#16114 = EDGE_CURVE ( 'NONE', #12899, #10958, #20290, .T. ) ;
#16115 = CYLINDRICAL_SURFACE ( 'NONE', #21009, 2.844799999999994444 ) ;
#16116 = DIRECTION ( 'NONE',  ( -1.000000000000000000, 0.000000000000000000, 0.000000000000000000 ) ) ;
#16117 = CARTESIAN_POINT ( 'NONE',  ( 25.39999999999999858, -3578.860000000000127, 2247.392000000000280 ) ) ;
#16118 = LOCAL_TIME ( 17, 37, 43.00000000000000000, #19804 ) ;
#16119 = PRODUCT_DEFINITION_FORMATION_WITH_SPECIFIED_SOURCE ( 'ANY', '', #5080, .NOT_KNOWN. ) ;
#16120 = ORIENTED_EDGE ( 'NONE', *, *, #13042, .T. ) ;
#16121 = CARTESIAN_POINT ( 'NONE',  ( -12.31900000000000084, -3581.552400000000034, 2247.392000000000280 ) ) ;
#16122 = EDGE_CURVE ( 'NONE', #3685, #13123, #3064, .T. ) ;
#16123 = CARTESIAN_POINT ( 'NONE',  ( 20.32000000000000028, -3694.938000000000102, 2289.213099999999940 ) ) ;
#16124 = CARTESIAN_POINT ( 'NONE',  ( 47.95519999999999783, -3619.500000000000000, 2239.771999999999935 ) ) ;
#16125 = CARTESIAN_POINT ( 'NONE',  ( 12.69999999999999929, -3583.940000000000055, 2268.705139999999574 ) ) ;
#16126 = PRODUCT_DEFINITION_SHAPE ( 'NONE', 'NONE',  #12365 ) ;
#16127 = CARTESIAN_POINT ( 'NONE',  ( 18.25163997286968254, -3658.148427273620200, 2245.360569998716983 ) ) ;
#16128 = ORIENTED_EDGE ( 'NONE', *, *, #8776, .T. ) ;
#16129 = CARTESIAN_POINT ( 'NONE',  ( -12.69999999999999929, -3580.426170452999941, 2250.104686796999886 ) ) ;
#16130 = B_SPLINE_CURVE_WITH_KNOTS ( 'NONE', 3,
 ( #3921, #7446, #3803, #183, #16231, #16348, #5584, #18330, #10957, #16571, #2398, #4042, #12944, #18102, #5813, #4152, #20103, #11188, #16455 ),
 .UNSPECIFIED., .F., .F.,
 ( 4, 2, 2, 1, 2, 2, 2, 2, 2, 4 ),
 ( 0.000000000000000000, 0.1249999999982433219, 0.1874999999975868747, 0.2187499999972586651, 0.2343749999970945463, 0.2499999999969304554, 0.3749999999975224818, 0.4999999999981145082, 0.7499999999990571986, 1.000000000000000000 ),
 .UNSPECIFIED. ) ;
#16131 = CARTESIAN_POINT ( 'NONE',  ( -6.350000000000118661, -3578.860000000000127, 2242.311999999999898 ) ) ;
#16132 = CARTESIAN_POINT ( 'NONE',  ( -12.69999999999999929, -3658.573829547000059, 2244.679313203000220 ) ) ;
#16133 = CARTESIAN_POINT ( 'NONE',  ( 142.0316867971961869, -3578.148799999863513, 2239.167815367201456 ) ) ;
#16134 = CARTESIAN_POINT ( 'NONE',  ( 0.000000000000000000, -3578.860000000000127, 2251.506800000000112 ) ) ;
#16135 = LOCAL_TIME ( 17, 37, 43.00000000000000000, #17899 ) ;
#16136 = ORIENTED_EDGE ( 'NONE', *, *, #17310, .T. ) ;
#16137 = LOCAL_TIME ( 17, 37, 43.00000000000000000, #10021 ) ;
#16138 = DIRECTION ( 'NONE',  ( 0.000000000000000000, -1.000000000000000000, 0.000000000000000000 ) ) ;
#16139 = ORIENTED_EDGE ( 'NONE', *, *, #6085, .T. ) ;
#16140 = EDGE_CURVE ( 'NONE', #11162, #2445, #13157, .T. ) ;
#16141 = DIRECTION ( 'NONE',  ( -1.000000000000000000, 0.000000000000000000, 0.000000000000000000 ) ) ;
#16142 = DIRECTION ( 'NONE',  ( -1.000000000000000000, 0.000000000000000000, 0.000000000000000000 ) ) ;
#16143 = TOROIDAL_SURFACE ( 'NONE', #10159, 4.114799999999999791, 1.270000000000000018 ) ;
#16144 = COORDINATED_UNIVERSAL_TIME_OFFSET ( 0, 0, .AHEAD. ) ;
#16145 = ADVANCED_FACE ( 'NONE', ( #10458 ), #9046, .T. ) ;
#16146 = CIRCLE ( 'NONE', #4520, 0.7619999999999987894 ) ;
#16147 = DIRECTION ( 'NONE',  ( -1.000000000000000000, 0.000000000000000000, 0.000000000000000000 ) ) ;
#16148 = EDGE_CURVE ( 'NONE', #17874, #22306, #3725, .T. ) ;
#16149 = LINE ( 'NONE', #94, #19847 ) ;
#16150 = LINE ( 'NONE', #3714, #6223 ) ;
#16151 = CARTESIAN_POINT ( 'NONE',  ( 3.048000000000000043, -3544.061999999999898, 2229.612000000000080 ) ) ;
#16152 = APPROVAL_PERSON_ORGANIZATION ( #20197, #17193, #4138 ) ;
#16153 = CARTESIAN_POINT ( 'NONE',  ( 25.39999999999999858, -3568.700000000000273, 2239.009999999999764 ) ) ;
#16154 = ORIENTED_EDGE ( 'NONE', *, *, #2411, .F. ) ;
#16155 = PLANE ( 'NONE',  #13693 ) ;
#16156 = FACE_OUTER_BOUND ( 'NONE', #9018, .T. ) ;
#16157 = ORIENTED_EDGE ( 'NONE', *, *, #5073, .F. ) ;
#16158 = CARTESIAN_POINT ( 'NONE',  ( 64.76999999999999602, -3543.299999999999727, 2285.606299999999919 ) ) ;
#16159 = AXIS2_PLACEMENT_3D ( 'NONE', #1312, #13863, #15741 ) ;
#16160 = ADVANCED_FACE ( 'NONE', ( #3308 ), #12452, .T. ) ;
#16161 = VECTOR ( 'NONE', #6714, 1000.000000000000000 ) ;
#16162 = ORIENTED_EDGE ( 'NONE', *, *, #13215, .F. ) ;
#16163 = CARTESIAN_POINT ( 'NONE',  ( -6.349999999999999645, -3660.140000000000327, 2247.392000000000280 ) ) ;
#16164 = LINE ( 'NONE', #16277, #3066 ) ;
#16165 = ORIENTED_EDGE ( 'NONE', *, *, #9000, .F. ) ;
#16166 = CARTESIAN_POINT ( 'NONE',  ( 137.9071795004996943, -3581.703785729057017, 2247.306121288057057 ) ) ;
#16167 = VERTEX_POINT ( 'NONE', #3657 ) ;
#16168 = PERSON_AND_ORGANIZATION_ROLE ( 'design_owner' ) ;
#16169 = EDGE_CURVE ( 'NONE', #15892, #6818, #797, .T. ) ;
#16170 = CARTESIAN_POINT ( 'NONE',  ( 142.2400000000000091, -3544.570000000000164, 2254.503999999999905 ) ) ;
#16171 = DIRECTION ( 'NONE',  ( 1.000000000000000000, 0.000000000000000000, 0.000000000000000000 ) ) ;
#16172 = B_SPLINE_CURVE_WITH_KNOTS ( 'NONE', 3,
 ( #6700, #6351, #15600, #2816 ),
 .UNSPECIFIED., .F., .F.,
 ( 4, 4 ),
 ( 0.000000000000000000, 1.000000000000000000 ),
 .UNSPECIFIED. ) ;
#16173 = CIRCLE ( 'NONE', #6076, 2.844799999999009010 ) ;
#16174 = CARTESIAN_POINT ( 'NONE',  ( 10.36831320285999958, -3658.158799999999701, 2242.820000000000164 ) ) ;
#16175 = CARTESIAN_POINT ( 'NONE',  ( 101.5999999999999943, -3619.500000000000000, 2259.837999999999738 ) ) ;
#16176 = AXIS2_PLACEMENT_3D ( 'NONE', #18144, #19678, #112 ) ;
#16177 = CARTESIAN_POINT ( 'NONE',  ( 142.1753987576898055, -3578.092974057908123, 2250.131498804146304 ) ) ;
#16178 = ORIENTED_EDGE ( 'NONE', *, *, #5208, .T. ) ;
#16179 = CARTESIAN_POINT ( 'NONE',  ( 134.2649038272905386, -3577.728047718949256, 2244.781081195526895 ) ) ;
#16180 = EDGE_LOOP ( 'NONE', ( #6080, #5136, #17651, #8947, #3748 ) ) ;
#16181 = LINE ( 'NONE', #3638, #17766 ) ;
#16182 = ORIENTED_EDGE ( 'NONE', *, *, #4797, .F. ) ;
#16183 = CARTESIAN_POINT ( 'NONE',  ( 9.904004635912999177, -3580.043455317999815, 2257.950092655999924 ) ) ;
#16184 = CARTESIAN_POINT ( 'NONE',  ( 19.05000000000000071, -3580.764999999999873, 2247.392000000000280 ) ) ;
#16185 = AXIS2_PLACEMENT_3D ( 'NONE', #9233, #6404, #15306 ) ;
#16186 = ADVANCED_FACE ( 'NONE', ( #23102 ), #7416, .T. ) ;
#16187 = VERTEX_POINT ( 'NONE', #14566 ) ;
#16188 = CARTESIAN_POINT ( 'NONE',  ( 15.54479972192533488, -3659.504999998566745, 2257.962943247991007 ) ) ;
#16189 = AXIS2_PLACEMENT_3D ( 'NONE', #11925, #6669, #22804 ) ;
#16190 = CARTESIAN_POINT ( 'NONE',  ( 15.87500000000000000, -3694.938000000000102, 2282.113800000000083 ) ) ;
#16191 = TOROIDAL_SURFACE ( 'NONE', #4944, 3.606799999999999784, 0.7620000000000000107 ) ;
#16192 = ORIENTED_EDGE ( 'NONE', *, *, #10815, .T. ) ;
#16193 = AXIS2_PLACEMENT_3D ( 'NONE', #11229, #2329, #18488 ) ;
#16194 = DIRECTION ( 'NONE',  ( 0.000000000000000000, 0.000000000000000000, 1.000000000000000000 ) ) ;
#16195 = CARTESIAN_POINT ( 'NONE',  ( 10.68406120964000117, -3641.518414594000205, 2279.634081700000479 ) ) ;
#16196 = LINE ( 'NONE', #147, #21792 ) ;
#16197 = DIRECTION ( 'NONE',  ( 0.000000000000000000, 0.000000000000000000, 1.000000000000000000 ) ) ;
#16198 = APPROVAL_STATUS ( 'not_yet_approved' ) ;
#16199 = CARTESIAN_POINT ( 'NONE',  ( 10.36831320284000135, -3598.151299999999992, 2292.781800000000203 ) ) ;
#16200 = DIRECTION ( 'NONE',  ( 0.000000000000000000, 1.000000000000000000, 0.000000000000000000 ) ) ;
#16201 = VERTEX_POINT ( 'NONE', #21706 ) ;
#16202 = CARTESIAN_POINT ( 'NONE',  ( 15.03168679714000078, -3640.848700000000008, 2296.210799999999836 ) ) ;
#16203 = VECTOR ( 'NONE', #22290, 1000.000000000000000 ) ;
#16204 = CARTESIAN_POINT ( 'NONE',  ( 22.55520000000100111, -3568.700000000000273, 2259.837999999999738 ) ) ;
#16205 = ORIENTED_EDGE ( 'NONE', *, *, #17026, .F. ) ;
#16206 = AXIS2_PLACEMENT_3D ( 'NONE', #20226, #83, #21754 ) ;
#16207 = CARTESIAN_POINT ( 'NONE',  ( 137.6831814252260813, -3661.513472532589276, 2249.884315932574737 ) ) ;
#16208 = ORIENTED_EDGE ( 'NONE', *, *, #12393, .F. ) ;
#16209 = ORIENTED_EDGE ( 'NONE', *, *, #18822, .T. ) ;
#16210 = ORIENTED_EDGE ( 'NONE', *, *, #11519, .T. ) ;
#16211 = CARTESIAN_POINT ( 'NONE',  ( 139.6999999999999886, -3659.504999999999654, 2244.978999999999814 ) ) ;
#16212 = VERTEX_POINT ( 'NONE', #10692 ) ;
#16213 = ORIENTED_EDGE ( 'NONE', *, *, #9181, .F. ) ;
#16214 = FACE_OUTER_BOUND ( 'NONE', #1157, .T. ) ;
#16215 = PERSON_AND_ORGANIZATION ( #2644, #21371 ) ;
#16216 = CARTESIAN_POINT ( 'NONE',  ( 139.6999999999999886, -3579.494999999999891, 2244.978999999999814 ) ) ;
#16217 = CIRCLE ( 'NONE', #12837, 2.844799999999994444 ) ;
#16218 = DIRECTION ( 'NONE',  ( 0.000000000000000000, 0.000000000000000000, 1.000000000000000000 ) ) ;
#16219 = VERTEX_POINT ( 'NONE', #19371 ) ;
#16220 = LINE ( 'NONE', #8961, #1749 ) ;
#16221 = CARTESIAN_POINT ( 'NONE',  ( 57.14999999999999858, -3543.299999999999727, 2247.392000000000280 ) ) ;
#16222 = CARTESIAN_POINT ( 'NONE',  ( 7.086979097592000620, -3580.606330658807565, 2245.129232553048496 ) ) ;
#16223 = DIRECTION ( 'NONE',  ( 0.000000000000000000, 0.000000000000000000, 1.000000000000000000 ) ) ;
#16224 = PERSON_AND_ORGANIZATION ( #5446, #1895 ) ;
#16225 = AXIS2_PLACEMENT_3D ( 'NONE', #22850, #17582, #8577 ) ;
#16226 = VERTEX_POINT ( 'NONE', #21480 ) ;
#16227 = CARTESIAN_POINT ( 'NONE',  ( 131.9328299862054905, -3543.675011529194762, 2260.231706197272615 ) ) ;
#16228 = EDGE_LOOP ( 'NONE', ( #15730, #13827, #10707, #8788 ) ) ;
#16229 = APPLIED_PERSON_AND_ORGANIZATION_ASSIGNMENT ( #8738, #21506, ( #13135 ) ) ;
#16230 = DIRECTION ( 'NONE',  ( -1.000000000000000000, 0.000000000000000000, 0.000000000000000000 ) ) ;
#16231 = CARTESIAN_POINT ( 'NONE',  ( 7.939941740107332002, -3662.668415385413937, 2246.085609779290280 ) ) ;
#16232 = ORIENTED_EDGE ( 'NONE', *, *, #17520, .F. ) ;
#16233 = VECTOR ( 'NONE', #3488, 1000.000000000000000 ) ;
#16234 = DIRECTION ( 'NONE',  ( 0.000000000000000000, 0.000000000000000000, 1.000000000000000000 ) ) ;
#16235 = EDGE_CURVE ( 'NONE', #1438, #14110, #12335, .T. ) ;
#16236 = EDGE_CURVE ( 'NONE', #12668, #6472, #6830, .T. ) ;
#16237 = FACE_OUTER_BOUND ( 'NONE', #3901, .T. ) ;
#16238 = DIRECTION ( 'NONE',  ( 1.000000000000000000, 0.000000000000000000, 0.000000000000000000 ) ) ;
#16239 = CARTESIAN_POINT ( 'NONE',  ( 1.270000000000000018, -3578.860000000000127, 2247.392000000000280 ) ) ;
#16240 = ADVANCED_FACE ( 'NONE', ( #3426, #10580 ), #17716, .F. ) ;
#16241 = CARTESIAN_POINT ( 'NONE',  ( 18.11755229430770697, -3657.685221718821140, 2245.954260265993980 ) ) ;
#16242 = VERTEX_POINT ( 'NONE', #15968 ) ;
#16243 = CYLINDRICAL_SURFACE ( 'NONE', #9755, 2.844799999999009010 ) ;
#16244 = CARTESIAN_POINT ( 'NONE',  ( 15.54479999999999862, -3599.497499999999945, 2279.447335734999797 ) ) ;
#16245 = CARTESIAN_POINT ( 'NONE',  ( 15.03168679710911704, -3660.851200000110111, 2239.391000000000076 ) ) ;
#16246 = LINE ( 'NONE', #14266, #12322 ) ;
#16247 = EDGE_CURVE ( 'NONE', #14745, #4174, #22526, .T. ) ;
#16248 = CARTESIAN_POINT ( 'NONE',  ( 136.9313810085959062, -3695.492037868740226, 2255.201647171010791 ) ) ;
#16249 = ORIENTED_EDGE ( 'NONE', *, *, #20451, .F. ) ;
#16250 = ORIENTED_EDGE ( 'NONE', *, *, #21985, .F. ) ;
#16251 = DATE_TIME_ROLE ( 'creation_date' ) ;
#16252 = CIRCLE ( 'NONE', #1268, 2.844800000000001550 ) ;
#16253 = DIRECTION ( 'NONE',  ( 0.000000000000000000, 1.000000000000000000, 0.000000000000000000 ) ) ;
#16254 = ORIENTED_EDGE ( 'NONE', *, *, #5511, .T. ) ;
#16255 = EDGE_CURVE ( 'NONE', #17585, #6642, #12945, .T. ) ;
#16256 = CARTESIAN_POINT ( 'NONE',  ( 12.69999999999999929, -3639.502500000000055, 2290.622800000000097 ) ) ;
#16257 = APPROVAL_STATUS ( 'not_yet_approved' ) ;
#16258 = CYLINDRICAL_SURFACE ( 'NONE', #17288, 1.269999999999882334 ) ;
#16259 = DIRECTION ( 'NONE',  ( -1.224646799147353207E-16, 1.000000000000000000, 0.000000000000000000 ) ) ;
#16260 = DIRECTION ( 'NONE',  ( 1.000000000000000000, -0.000000000000000000, 1.224646799147353207E-16 ) ) ;
#16261 = CARTESIAN_POINT ( 'NONE',  ( 101.5999999999999943, -3568.700000000000273, 2261.869999999999891 ) ) ;
#16262 = EDGE_CURVE ( 'NONE', #19268, #8944, #4121, .T. ) ;
#16263 = ORIENTED_EDGE ( 'NONE', *, *, #14838, .F. ) ;
#16264 = FACE_BOUND ( 'NONE', #19844, .T. ) ;
#16265 = ORIENTED_EDGE ( 'NONE', *, *, #11943, .T. ) ;
#16266 = AXIS2_PLACEMENT_3D ( 'NONE', #10762, #12985, #18360 ) ;
#16267 = EDGE_CURVE ( 'NONE', #16307, #1882, #2254, .T. ) ;
#16268 = DIRECTION ( 'NONE',  ( 0.000000000000000000, 0.000000000000000000, -1.000000000000000000 ) ) ;
#16270 = ADVANCED_FACE ( 'NONE', ( #18415 ), #16191, .T. ) ;
#16269 = AXIS2_PLACEMENT_3D ( 'NONE', #16464, #19875, #10964 ) ;
#16271 = CARTESIAN_POINT ( 'NONE',  ( 10.68380249261999992, -3637.486841245000505, 2279.634034043999691 ) ) ;
#16272 = AXIS2_PLACEMENT_3D ( 'NONE', #14120, #15872, #22654 ) ;
#16273 = ORIENTED_EDGE ( 'NONE', *, *, #343, .T. ) ;
#16274 = CARTESIAN_POINT ( 'NONE',  ( 25.39999999999999858, -3660.140000000000327, 2247.392000000000280 ) ) ;
#16275 = VERTEX_POINT ( 'NONE', #9405 ) ;
#16276 = CARTESIAN_POINT ( 'NONE',  ( 142.2429993025672275, -3694.590198013145255, 2255.766426251082976 ) ) ;
#16277 = CARTESIAN_POINT ( 'NONE',  ( 0.7620000000000000107, -3695.699999999999818, 2295.829799999999977 ) ) ;
#16278 = ORIENTED_EDGE ( 'NONE', *, *, #1116, .T. ) ;
#16279 = CARTESIAN_POINT ( 'NONE',  ( 137.8421157351343709, -3581.650442338845551, 2246.808394885380039 ) ) ;
#16280 = VECTOR ( 'NONE', #2623, 1000.000000000000000 ) ;
#16281 = VERTEX_POINT ( 'NONE', #5660 ) ;
#16282 = CARTESIAN_POINT ( 'NONE',  ( 139.5113019466200228, -3582.339796537331949, 2257.592643468492042 ) ) ;
#16283 = PERSON_AND_ORGANIZATION ( #5446, #1895 ) ;
#16284 = AXIS2_PLACEMENT_3D ( 'NONE', #8780, #3612, #15929 ) ;
#16285 = AXIS2_PLACEMENT_3D ( 'NONE', #20764, #3300, #15844 ) ;
#16286 = DIRECTION ( 'NONE',  ( 0.000000000000000000, 1.000000000000000000, 0.000000000000000000 ) ) ;
#16287 = CARTESIAN_POINT ( 'NONE',  ( -0.7620000000000000107, -3694.938000000000102, 2254.250000000000000 ) ) ;
#16288 = DIRECTION ( 'NONE',  ( 1.206643234470999950E-12, -1.000000000000000000, -2.336881798973999985E-14 ) ) ;
#16289 = CARTESIAN_POINT ( 'NONE',  ( 105.2067999999999870, -3670.300000000000182, 2259.837999999999738 ) ) ;
#16290 = CARTESIAN_POINT ( 'NONE',  ( 138.0864475737284067, -3577.151256281058068, 2249.666874368690515 ) ) ;
#16291 = EDGE_LOOP ( 'NONE', ( #16080, #4224, #11411, #19799 ) ) ;
#16292 = CARTESIAN_POINT ( 'NONE',  ( 134.0205977155505650, -3578.857768333618878, 2244.547199809527683 ) ) ;
#16293 = CARTESIAN_POINT ( 'NONE',  ( 12.70000000000000107, -3648.710000000000036, 2275.817139999999654 ) ) ;
#16294 = EDGE_LOOP ( 'NONE', ( #365, #6517 ) ) ;
#16295 = AXIS2_PLACEMENT_3D ( 'NONE', #23115, #16098, #46 ) ;
#16296 = CARTESIAN_POINT ( 'NONE',  ( 10.36831320285999958, -3578.148799999999937, 2239.391000000000076 ) ) ;
#16297 = CYLINDRICAL_SURFACE ( 'NONE', #2010, 2.844800000000091700 ) ;
#16298 = CIRCLE ( 'NONE', #9196, 5.460999999999938126 ) ;
#16299 = EDGE_CURVE ( 'NONE', #11298, #10072, #14325, .T. ) ;
#16300 = EDGE_CURVE ( 'NONE', #19963, #1715, #20573, .T. ) ;
#16301 = CIRCLE ( 'NONE', #1720, 0.7619999999999987894 ) ;
#16302 = ORIENTED_EDGE ( 'NONE', *, *, #17127, .T. ) ;
#16303 = EDGE_CURVE ( 'NONE', #3840, #11610, #11378, .T. ) ;
#16304 = DIRECTION ( 'NONE',  ( 0.000000000000000000, -0.8660254037840939834, -0.5000000000005969669 ) ) ;
#16305 = CARTESIAN_POINT ( 'NONE',  ( 95.25000000000000000, -3670.300000000000182, 2247.392000000000280 ) ) ;
#16306 = CIRCLE ( 'NONE', #1320, 2.844800000000001550 ) ;
#16307 = VERTEX_POINT ( 'NONE', #20296 ) ;
#16308 = CARTESIAN_POINT ( 'NONE',  ( 151.1299999999999955, -3695.699999999999818, 2259.329999999999927 ) ) ;
#16309 = DIRECTION ( 'NONE',  ( 1.000000000000000000, 0.000000000000000000, 0.000000000000000000 ) ) ;
#16310 = CARTESIAN_POINT ( 'NONE',  ( 57.14999999999999858, -3568.700000000000273, 2247.392000000000280 ) ) ;
#16311 = ADVANCED_FACE ( 'NONE', ( #9510 ), #8302, .F. ) ;
#16312 = DATE_AND_TIME ( #8935, #2256 ) ;
#16313 = DIRECTION ( 'NONE',  ( -1.711270818677000004E-12, 1.000000000000000000, -3.793660610079000032E-12 ) ) ;
#16314 = CARTESIAN_POINT ( 'NONE',  ( 9.971147940439486490, -3695.419680868843443, 2255.300839618168538 ) ) ;
#16315 = ORIENTED_EDGE ( 'NONE', *, *, #5008, .F. ) ;
#16316 = CARTESIAN_POINT ( 'NONE',  ( 18.14575475405891680, -3581.228764778724781, 2245.816281745348988 ) ) ;
#16317 = AXIS2_PLACEMENT_3D ( 'NONE', #15785, #19185, #20941 ) ;
#16318 = VECTOR ( 'NONE', #14025, 1000.000000000000114 ) ;
#16319 = ADVANCED_FACE ( 'NONE', ( #18841 ), #16652, .F. ) ;
#16320 = PRODUCT ( 'MAT-035', 'MAT-035', '', ( #11593 ) ) ;
#16321 = CARTESIAN_POINT ( 'NONE',  ( -6.349999999999999645, -3654.679000000000087, 2247.392000000000280 ) ) ;
#16322 = CIRCLE ( 'NONE', #22658, 1.269999999999882334 ) ;
#16323 = EDGE_CURVE ( 'NONE', #17137, #16091, #10192, .T. ) ;
#16324 = VERTEX_POINT ( 'NONE', #7523 ) ;
#16325 = ORIENTED_EDGE ( 'NONE', *, *, #1967, .F. ) ;
#16326 = AXIS2_PLACEMENT_3D ( 'NONE', #20567, #15309, #2996 ) ;
#16327 = CARTESIAN_POINT ( 'NONE',  ( 140.6722870908654386, -3662.179796010951577, 2249.375424445521730 ) ) ;
#16328 = AXIS2_PLACEMENT_3D ( 'NONE', #1400, #13831, #17329 ) ;
#16329 = AXIS2_PLACEMENT_3D ( 'NONE', #5349, #3579, #17881 ) ;
#16330 = EDGE_LOOP ( 'NONE', ( #2139, #2212, #7498, #2485, #6545, #6025, #10001, #477, #5671 ) ) ;
#16331 = ORIENTED_EDGE ( 'NONE', *, *, #21864, .T. ) ;
#16332 = CARTESIAN_POINT ( 'NONE',  ( 41.70680000000000121, -3644.899999999999636, 2259.837999999999738 ) ) ;
#16333 = ORIENTED_EDGE ( 'NONE', *, *, #18850, .F. ) ;
#16334 = EDGE_LOOP ( 'NONE', ( #3403, #16572, #9060, #12798 ) ) ;
#16335 = CARTESIAN_POINT ( 'NONE',  ( 0.000000000000000000, -3694.430000000000291, 2259.329999999999927 ) ) ;
#16336 = CARTESIAN_POINT ( 'NONE',  ( 142.0316867971999955, -3658.158799999999701, 2242.820000000000164 ) ) ;
#16337 = EDGE_LOOP ( 'NONE', ( #4986, #6980, #11760, #14026 ) ) ;
#16338 = CIRCLE ( 'NONE', #6243, 3.606799999998994366 ) ;
#16339 = CARTESIAN_POINT ( 'NONE',  ( 79.80679999999999552, -3670.300000000000182, 2239.009999999999764 ) ) ;
#16340 = DIRECTION ( 'NONE',  ( -1.000000000000000000, 0.000000000000000000, 0.000000000000000000 ) ) ;
#16341 = CARTESIAN_POINT ( 'NONE',  ( 0.000000000000000000, -3694.938000000000102, 2239.771999999999935 ) ) ;
#16342 = DIRECTION ( 'NONE',  ( 0.000000000000000000, 0.000000000000000000, -1.000000000000000000 ) ) ;
#16343 = PERSON_AND_ORGANIZATION_ROLE ( 'creator' ) ;
#16344 = AXIS2_PLACEMENT_3D ( 'NONE', #7000, #3462, #10263 ) ;
#16345 = CARTESIAN_POINT ( 'NONE',  ( 131.9608861896474252, -3543.750038107418732, 2260.302253161996305 ) ) ;
#16346 = VERTEX_POINT ( 'NONE', #10048 ) ;
#16347 = DIRECTION ( 'NONE',  ( 0.000000000000000000, 0.000000000000000000, -1.000000000000000000 ) ) ;
#16348 = CARTESIAN_POINT ( 'NONE',  ( 7.901418343680338019, -3662.609162415918490, 2245.978569001930282 ) ) ;
#16349 = FACE_OUTER_BOUND ( 'NONE', #17958, .T. ) ;
#16350 = ORIENTED_EDGE ( 'NONE', *, *, #22250, .T. ) ;
#16351 = FACE_OUTER_BOUND ( 'NONE', #20684, .T. ) ;
#16352 = DIRECTION ( 'NONE',  ( 0.000000000000000000, -1.000000000000000000, 0.000000000000000000 ) ) ;
#16353 = VECTOR ( 'NONE', #16747, 1000.000000000000000 ) ;
#16354 = CARTESIAN_POINT ( 'NONE',  ( 47.19319999999999737, -3670.300000000000182, 2239.771999999999935 ) ) ;
#16355 = DIRECTION ( 'NONE',  ( 0.000000000000000000, 0.000000000000000000, -1.000000000000000000 ) ) ;
#16356 = ORIENTED_EDGE ( 'NONE', *, *, #2260, .T. ) ;
#16357 = CARTESIAN_POINT ( 'NONE',  ( 18.03944995089040049, -3657.466237342172008, 2246.412073519087699 ) ) ;
#16358 = AXIS2_PLACEMENT_3D ( 'NONE', #307, #7451, #14604 ) ;
#16359 = VERTEX_POINT ( 'NONE', #11161 ) ;
#16360 = CARTESIAN_POINT ( 'NONE',  ( 147.6747367346642932, -3695.644174308748461, 2259.712265308950464 ) ) ;
#16361 = CYLINDRICAL_SURFACE ( 'NONE', #3905, 2.844799999999999773 ) ;
#16362 = DIRECTION ( 'NONE',  ( 0.000000000000000000, -1.000000000000000000, 0.000000000000000000 ) ) ;
#16363 = APPROVAL ( #13836, 'UNSPECIFIED' ) ;
#16364 = CARTESIAN_POINT ( 'NONE',  ( 4.572920519510999426, -3695.699999999999818, 2259.329999999999927 ) ) ;
#16365 = CARTESIAN_POINT ( 'NONE',  ( 136.9721883683046997, -3695.420022019528915, 2255.303812753265902 ) ) ;
#16366 = CARTESIAN_POINT ( 'NONE',  ( 7.834124089763437659, -3576.497611619219697, 2245.807063631086294 ) ) ;
#16367 = ORIENTED_EDGE ( 'NONE', *, *, #15390, .F. ) ;
#16368 = APPLICATION_PROTOCOL_DEFINITION ( 'international standard', 'automotive_design', 2000, #7232 ) ;
#16369 = AXIS2_PLACEMENT_3D ( 'NONE', #603, #9844, #6120 ) ;
#16370 = ADVANCED_FACE ( 'NONE', ( #17194 ), #18186, .F. ) ;
#16371 = CARTESIAN_POINT ( 'NONE',  ( 64.76999999999999602, -3568.700000000000273, 2289.213099999999940 ) ) ;
#16372 = DIRECTION ( 'NONE',  ( 0.000000000000000000, 0.000000000000000000, -1.000000000000000000 ) ) ;
#16373 = PERSON_AND_ORGANIZATION ( #10200, #779 ) ;
#16374 = ADVANCED_FACE ( 'NONE', ( #19954 ), #18300, .F. ) ;
#16375 = AXIS2_PLACEMENT_3D ( 'NONE', #1741, #1610, #6903 ) ;
#16376 = CARTESIAN_POINT ( 'NONE',  ( 7.619999999999999218, -3639.502500000000055, 2296.210799999999836 ) ) ;
#16377 = AXIS2_PLACEMENT_3D ( 'NONE', #17841, #8937, #21252 ) ;
#16378 = DIRECTION ( 'NONE',  ( -1.224646799141892071E-16, -1.000000000000000000, 2.336881798971000421E-14 ) ) ;
#16379 = DIRECTION ( 'NONE',  ( 0.000000000000000000, 0.000000000000000000, 1.000000000000000000 ) ) ;
#16380 = VERTEX_POINT ( 'NONE', #20073 ) ;
#16381 = PLANE ( 'NONE',  #21856 ) ;
#16382 = ORIENTED_EDGE ( 'NONE', *, *, #16604, .T. ) ;
#16383 = CARTESIAN_POINT ( 'NONE',  ( 18.01287425286000143, -3581.600847139000052, 2246.630000000000109 ) ) ;
#16384 = AXIS2_PLACEMENT_3D ( 'NONE', #22288, #15277, #22402 ) ;
#16385 = CARTESIAN_POINT ( 'NONE',  ( 12.31593207299000170, -3694.430000000000291, 2251.974139024000124 ) ) ;
#16386 = ORIENTED_EDGE ( 'NONE', *, *, #8593, .T. ) ;
#16387 = CYLINDRICAL_SURFACE ( 'NONE', #21546, 2.844800000000091700 ) ;
#16388 = EDGE_LOOP ( 'NONE', ( #13802, #18760, #973, #20765 ) ) ;
#16389 = CARTESIAN_POINT ( 'NONE',  ( 142.4276778852931784, -3695.420022016050098, 2255.303759356630508 ) ) ;
#16390 = DIRECTION ( 'NONE',  ( 1.000000000000000000, 0.000000000000000000, 0.000000000000000000 ) ) ;
#16391 = ORIENTED_EDGE ( 'NONE', *, *, #17954, .F. ) ;
#16392 = ADVANCED_FACE ( 'NONE', ( #493 ), #9802, .T. ) ;
#16393 = CARTESIAN_POINT ( 'NONE',  ( 137.7588963307679251, -3581.574831038090906, 2248.242363506559286 ) ) ;
#16394 = EDGE_LOOP ( 'NONE', ( #16768, #9062 ) ) ;
#16395 = CARTESIAN_POINT ( 'NONE',  ( 9.987313202833000503, -3639.502500000000055, 2296.210799999999836 ) ) ;
#16396 = EDGE_CURVE ( 'NONE', #2028, #16242, #15804, .T. ) ;
#16397 = APPLICATION_PROTOCOL_DEFINITION ( 'international standard', 'automotive_design', 2000, #19647 ) ;
#16398 = ADVANCED_FACE ( 'NONE', ( #12285 ), #103, .T. ) ;
#16399 = CIRCLE ( 'NONE', #997, 0.7619999999999294005 ) ;
#16400 = DIRECTION ( 'NONE',  ( 0.000000000000000000, 0.000000000000000000, -1.000000000000000000 ) ) ;
#16401 = CARTESIAN_POINT ( 'NONE',  ( 136.9873132028999976, -3659.504999999999654, 2239.391000000000076 ) ) ;
#16402 = CARTESIAN_POINT ( 'NONE',  ( 131.8084957954999936, -3544.527728344000025, 2260.600000000000364 ) ) ;
#16403 = CARTESIAN_POINT ( 'NONE',  ( 12.42449270472999956, -3576.659101290000308, 2257.594923725999706 ) ) ;
#16404 = CARTESIAN_POINT ( 'NONE',  ( 140.5570903332553030, -3576.782304280421613, 2249.335231873303655 ) ) ;
#16405 = ORIENTED_EDGE ( 'NONE', *, *, #9831, .F. ) ;
#16406 = CARTESIAN_POINT ( 'NONE',  ( 105.2067999999999870, -3619.500000000000000, 2239.009999999999764 ) ) ;
#16407 = DIRECTION ( 'NONE',  ( 1.000000000000000000, 0.000000000000000000, 0.000000000000000000 ) ) ;
#16408 = ORIENTED_EDGE ( 'NONE', *, *, #14891, .T. ) ;
#16409 = EDGE_CURVE ( 'NONE', #8256, #2597, #5252, .T. ) ;
#16410 = DIRECTION ( 'NONE',  ( 1.278298683861999854E-12, -1.000000000000000000, 0.000000000000000000 ) ) ;
#16411 = DIRECTION ( 'NONE',  ( -2.324635735433000053E-14, 0.000000000000000000, -1.000000000000000000 ) ) ;
#16412 = ORIENTED_EDGE ( 'NONE', *, *, #3509, .F. ) ;
#16413 = CARTESIAN_POINT ( 'NONE',  ( 12.70000020906999971, -3662.349800009999854, 2257.592639999999847 ) ) ;
#16414 = FACE_OUTER_BOUND ( 'NONE', #11196, .T. ) ;
#16415 = AXIS2_PLACEMENT_3D ( 'NONE', #10038, #21185, #10155 ) ;
#16416 = ORIENTED_EDGE ( 'NONE', *, *, #23095, .T. ) ;
#16417 = CARTESIAN_POINT ( 'NONE',  ( 139.6999999999999886, -3662.349799999999050, 2257.592639999999847 ) ) ;
#16418 = FACE_OUTER_BOUND ( 'NONE', #1803, .T. ) ;
#16419 =( NAMED_UNIT ( * ) SI_UNIT ( $, .STERADIAN. ) SOLID_ANGLE_UNIT ( ) );
#16420 = CARTESIAN_POINT ( 'NONE',  ( 7.619999999999999218, -3599.497499999999945, 2290.622800000000097 ) ) ;
#16421 = ORIENTED_EDGE ( 'NONE', *, *, #343, .F. ) ;
#16422 = CARTESIAN_POINT ( 'NONE',  ( 21.79320000000099711, -3568.700000000000273, 2239.009999999999764 ) ) ;
#16423 = DATE_TIME_ROLE ( 'creation_date' ) ;
#16424 = EDGE_CURVE ( 'NONE', #18606, #18259, #3081, .T. ) ;
#16425 = PLANE ( 'NONE',  #19746 ) ;
#16426 = DIRECTION ( 'NONE',  ( 0.000000000000000000, 0.000000000000000000, -1.000000000000000000 ) ) ;
#16427 = ORIENTED_EDGE ( 'NONE', *, *, #956, .T. ) ;
#16428 = CARTESIAN_POINT ( 'NONE',  ( 18.01287425286000143, -3581.600847139000052, 2246.630000000000109 ) ) ;
#16429 = EDGE_CURVE ( 'NONE', #18286, #1414, #1736, .T. ) ;
#16430 = DIRECTION ( 'NONE',  ( 0.000000000000000000, -1.000000000000000000, 0.000000000000000000 ) ) ;
#16431 = ADVANCED_FACE ( 'NONE', ( #12162 ), #3483, .F. ) ;
#16432 = ORIENTED_EDGE ( 'NONE', *, *, #14533, .T. ) ;
#16433 = CIRCLE ( 'NONE', #7839, 6.477000000000000313 ) ;
#16434 = CARTESIAN_POINT ( 'NONE',  ( 138.8069558488828932, -3662.206088545077819, 2249.347568272374701 ) ) ;
#16435 = VERTEX_POINT ( 'NONE', #21310 ) ;
#16436 = EDGE_CURVE ( 'NONE', #7405, #10930, #4896, .T. ) ;
#16437 = EDGE_LOOP ( 'NONE', ( #22745, #17739 ) ) ;
#16438 = DIRECTION ( 'NONE',  ( 0.000000000000000000, 0.000000000000000000, -1.000000000000000000 ) ) ;
#16439 = ORIENTED_EDGE ( 'NONE', *, *, #5272, .F. ) ;
#16440 = ORIENTED_EDGE ( 'NONE', *, *, #19258, .T. ) ;
#16441 = CARTESIAN_POINT ( 'NONE',  ( 15.24000000000000021, -3658.223872745999870, 2255.774000000000342 ) ) ;
#16442 = CARTESIAN_POINT ( 'NONE',  ( 101.5999999999999943, -3619.500000000000000, 2239.771999999999935 ) ) ;
#16443 = EDGE_CURVE ( 'NONE', #14575, #4022, #20837, .T. ) ;
#16444 = EDGE_LOOP ( 'NONE', ( #2830, #21607, #8600, #9250 ) ) ;
#16445 = LINE ( 'NONE', #14356, #15586 ) ;
#16446 = EDGE_CURVE ( 'NONE', #8260, #9227, #11667, .T. ) ;
#16447 = CARTESIAN_POINT ( 'NONE',  ( 7.306649500355966609, -3581.385628413785980, 2246.082317946663352 ) ) ;
#16448 = CARTESIAN_POINT ( 'NONE',  ( 95.25000000000000000, -3694.430000000000291, 2247.392000000000280 ) ) ;
#16449 = PERSON_AND_ORGANIZATION_ROLE ( 'classification_officer' ) ;
#16450 = LINE ( 'NONE', #9534, #6063 ) ;
#16451 = EDGE_LOOP ( 'NONE', ( #16895, #3931, #6562, #15636, #8394 ) ) ;
#16452 = DIRECTION ( 'NONE',  ( 1.000000000000000000, 0.000000000000000000, 0.000000000000000000 ) ) ;
#16453 = ADVANCED_FACE ( 'NONE', ( #17423 ), #14041, .T. ) ;
#16454 = EDGE_LOOP ( 'NONE', ( #6915, #19578, #5037, #22475 ) ) ;
#16455 = CARTESIAN_POINT ( 'NONE',  ( 7.020566483207999475, -3660.139755500999854, 2244.547200037999573 ) ) ;
#16456 = DIRECTION ( 'NONE',  ( -1.000000000000000000, 2.330758767201999921E-14, 2.356218894535000080E-14 ) ) ;
#16457 = EDGE_LOOP ( 'NONE', ( #6852, #842 ) ) ;
#16458 = CARTESIAN_POINT ( 'NONE',  ( 15.41268679715999923, -3657.938829547000296, 2239.009999999999764 ) ) ;
#16459 = AXIS2_PLACEMENT_3D ( 'NONE', #18269, #20267, #18154 ) ;
#16460 = LOCAL_TIME ( 17, 37, 43.00000000000000000, #5779 ) ;
#16461 = CARTESIAN_POINT ( 'NONE',  ( 63.50000000000000000, -3644.899999999999636, 2239.771999999999935 ) ) ;
#16462 =( GEOMETRIC_REPRESENTATION_CONTEXT ( 3 ) GLOBAL_UNCERTAINTY_ASSIGNED_CONTEXT ( ( #9258 ) ) GLOBAL_UNIT_ASSIGNED_CONTEXT ( ( #17942, #17480, #21592 ) ) REPRESENTATION_CONTEXT ( 'NONE', 'WORKASPACE' ) );
#16463 = CARTESIAN_POINT ( 'NONE',  ( 12.69999999999999929, -3599.497499999999945, 2264.841800000000148 ) ) ;
#16464 = CARTESIAN_POINT ( 'NONE',  ( 139.6999999999999886, -3579.494999999999891, 2244.978999999999814 ) ) ;
#16465 = ORIENTED_EDGE ( 'NONE', *, *, #9713, .T. ) ;
#16466 = CARTESIAN_POINT ( 'NONE',  ( 18.16341182905199503, -3657.827357193916214, 2245.734039593747639 ) ) ;
#16467 = ORIENTED_EDGE ( 'NONE', *, *, #5955, .F. ) ;
#16468 = CARTESIAN_POINT ( 'NONE',  ( 139.6999999999999886, -3579.494999999999891, 2272.030000000000200 ) ) ;
#16469 = CARTESIAN_POINT ( 'NONE',  ( 15.03168679710029743, -3578.148799999889434, 2239.391000000000076 ) ) ;
#16470 = CARTESIAN_POINT ( 'NONE',  ( 29.00679999999900005, -3670.300000000000182, 2260.600000000000364 ) ) ;
#16471 = EDGE_CURVE ( 'NONE', #1593, #8560, #7944, .T. ) ;
#16472 = CARTESIAN_POINT ( 'NONE',  ( 127.0000000000000000, -3578.860000000000127, 2247.392000000000280 ) ) ;
#16473 = DIRECTION ( 'NONE',  ( 0.000000000000000000, 0.000000000000000000, 1.000000000000000000 ) ) ;
#16474 = CARTESIAN_POINT ( 'NONE',  ( 10.36831320293767078, -3658.158799999985604, 2239.391000000000076 ) ) ;
#16475 = CARTESIAN_POINT ( 'NONE',  ( 7.579779957786826117, -3576.956500483505806, 2245.277209879519887 ) ) ;
#16476 = EDGE_LOOP ( 'NONE', ( #17414, #11215 ) ) ;
#16478 = TOROIDAL_SURFACE ( 'NONE', #12364, 3.606799999998999695, 0.7620000000000000107 ) ;
#16477 = DATE_AND_TIME ( #14618, #1503 ) ;
#16479 = ORIENTED_EDGE ( 'NONE', *, *, #20679, .F. ) ;
#16480 = CARTESIAN_POINT ( 'NONE',  ( -12.31900000000000084, -3658.793799999878502, 2245.060313203211081 ) ) ;
#16481 = SECURITY_CLASSIFICATION ( '', '', #15564 ) ;
#16482 = APPROVAL_PERSON_ORGANIZATION ( #21160, #1616, #19163 ) ;
#16483 = CARTESIAN_POINT ( 'NONE',  ( -8.890000000017000303, -3658.793800000000374, 2249.723686796999573 ) ) ;
#16484 = CARTESIAN_POINT ( 'NONE',  ( 41.70680000000000121, -3594.099999999999909, 2239.771999999999935 ) ) ;
#16485 = DIRECTION ( 'NONE',  ( -1.000000000000000000, 2.318894227180000040E-14, 2.343004830739999973E-14 ) ) ;
#16486 = CIRCLE ( 'NONE', #10870, 0.7619999999999294005 ) ;
#16487 = CARTESIAN_POINT ( 'NONE',  ( 134.9639022863356388, -3662.704503798480346, 2246.158276165796451 ) ) ;
#16488 = APPROVAL ( #3830, 'UNKNOWN' ) ;
#16489 = ORIENTED_EDGE ( 'NONE', *, *, #4200, .F. ) ;
#16490 = DIRECTION ( 'NONE',  ( -1.000000000000000000, 5.461016542361937364E-28, 2.336881798970999789E-14 ) ) ;
#16491 = ORIENTED_EDGE ( 'NONE', *, *, #23005, .F. ) ;
#16492 = DIRECTION ( 'NONE',  ( -2.170301461641000033E-13, -2.590196616223999907E-13, -1.000000000000000000 ) ) ;
#16493 = LINE ( 'NONE', #14750, #12198 ) ;
#16494 = ORIENTED_EDGE ( 'NONE', *, *, #3219, .T. ) ;
#16495 = APPLIED_SECURITY_CLASSIFICATION_ASSIGNMENT ( #16852, ( #23171 ) ) ;
#16496 = DIRECTION ( 'NONE',  ( 0.000000000000000000, 0.000000000000000000, -1.000000000000000000 ) ) ;
#16497 = LOCAL_TIME ( 17, 37, 43.00000000000000000, #9426 ) ;
#16498 = CARTESIAN_POINT ( 'NONE',  ( 1.270000000000000018, -3544.570000000000164, 2259.329999999999927 ) ) ;
#16499 = ORIENTED_EDGE ( 'NONE', *, *, #211, .F. ) ;
#16500 = CYLINDRICAL_SURFACE ( 'NONE', #19415, 0.3809999999999647002 ) ;
#16501 = CARTESIAN_POINT ( 'NONE',  ( 1.270000000000000018, -3578.860000000000127, 2251.506800000000112 ) ) ;
#16502 = ORIENTED_EDGE ( 'NONE', *, *, #22802, .T. ) ;
#16503 = AXIS2_PLACEMENT_3D ( 'NONE', #6506, #6281, #20663 ) ;
#16504 = UNCERTAINTY_MEASURE_WITH_UNIT (LENGTH_MEASURE( 1.000000000000000082E-05 ), #20317, 'distance_accuracy_value', 'NONE');
#16505 = VERTEX_POINT ( 'NONE', #4784 ) ;
#16506 = CARTESIAN_POINT ( 'NONE',  ( 145.2441493676143409, -3580.882459096562343, 2245.390311603773625 ) ) ;
#16507 = CALENDAR_DATE ( 2026, 26, 10 ) ;
#16508 = CARTESIAN_POINT ( 'NONE',  ( 57.14999999999999858, -3568.700000000000273, 2244.547199999999975 ) ) ;
#16509 = DIRECTION ( 'NONE',  ( 0.000000000000000000, 1.000000000000000000, 0.000000000000000000 ) ) ;
#16510 = DIRECTION ( 'NONE',  ( 0.000000000000000000, -1.000000000000000000, 0.000000000000000000 ) ) ;
#16511 = APPLIED_PERSON_AND_ORGANIZATION_ASSIGNMENT ( #3331, #17628, ( #11226 ) ) ;
#16512 = DIRECTION ( 'NONE',  ( 1.000000000000000000, 0.000000000000000000, 0.000000000000000000 ) ) ;
#16513 = CARTESIAN_POINT ( 'NONE',  ( 138.9527035083802105, -3576.750047203152462, 2249.300150270811173 ) ) ;
#16514 = EDGE_LOOP ( 'NONE', ( #16912, #21085, #17914 ) ) ;
#16515 = CIRCLE ( 'NONE', #12411, 1.269999999999882334 ) ;
#16516 = CIRCLE ( 'NONE', #6799, 0.7619999999999294005 ) ;
#16517 = ADVANCED_FACE ( 'NONE', ( #8542 ), #3255, .F. ) ;
#16518 = VERTEX_POINT ( 'NONE', #11928 ) ;
#16519 = CARTESIAN_POINT ( 'NONE',  ( 145.0128742528999908, -3581.600847139000052, 2246.630000000000109 ) ) ;
#16520 = ORIENTED_EDGE ( 'NONE', *, *, #1493, .T. ) ;
#16521 = EDGE_CURVE ( 'NONE', #19453, #22298, #21195, .T. ) ;
#16522 = CARTESIAN_POINT ( 'NONE',  ( 142.2400000000000091, -3695.699999999999818, 2255.774000000000342 ) ) ;
#16523 = CARTESIAN_POINT ( 'NONE',  ( 15.55234650392334927, -3543.397347667163558, 2254.991636092748649 ) ) ;
#16524 = EDGE_CURVE ( 'NONE', #1541, #21716, #17295, .T. ) ;
#16525 = ORIENTED_EDGE ( 'NONE', *, *, #15898, .F. ) ;
#16526 = CARTESIAN_POINT ( 'NONE',  ( 13.51841762737000074, -3662.234253382000134, 2257.621745511999961 ) ) ;
#16527 = DIRECTION ( 'NONE',  ( 0.000000000000000000, 0.000000000000000000, 1.000000000000000000 ) ) ;
#16528 = EDGE_LOOP ( 'NONE', ( #20337, #18149 ) ) ;
#16529 = FACE_OUTER_BOUND ( 'NONE', #12750, .T. ) ;
#16530 = CARTESIAN_POINT ( 'NONE',  ( 15.15611746081473399, -3578.059478917778051, 2250.121899032252259 ) ) ;
#16531 = DIRECTION ( 'NONE',  ( 0.000000000000000000, 0.000000000000000000, 1.000000000000000000 ) ) ;
#16532 = ADVANCED_FACE ( 'NONE', ( #8417 ), #6783, .T. ) ;
#16533 = DIRECTION ( 'NONE',  ( 1.000000000000000000, 0.000000000000000000, 0.000000000000000000 ) ) ;
#16534 = VERTEX_POINT ( 'NONE', #13923 ) ;
#16536 = CARTESIAN_POINT ( 'NONE',  ( 92.50679999999999836, -3594.099999999999909, 2259.837999999999738 ) ) ;
#16535 = AXIS2_PLACEMENT_3D ( 'NONE', #21508, #5338, #2174 ) ;
#16537 = CALENDAR_DATE ( 2026, 26, 10 ) ;
#16538 = AXIS2_PLACEMENT_3D ( 'NONE', #22141, #924, #22027 ) ;
#16539 = DIRECTION ( 'NONE',  ( 0.000000000000000000, 0.000000000000000000, 1.000000000000000000 ) ) ;
#16540 = DIRECTION ( 'NONE',  ( 0.000000000000000000, -1.000000000000000000, 0.000000000000000000 ) ) ;
#16541 = ORIENTED_EDGE ( 'NONE', *, *, #2300, .T. ) ;
#16542 = CARTESIAN_POINT ( 'NONE',  ( 18.24414936330329340, -3580.882459114104677, 2245.390311621496039 ) ) ;
#16543 = ADVANCED_FACE ( 'NONE', ( #21073 ), #6900, .F. ) ;
#16544 = DIRECTION ( 'NONE',  ( 0.000000000000000000, 0.000000000000000000, -1.000000000000000000 ) ) ;
#16545 = ORIENTED_EDGE ( 'NONE', *, *, #6952, .F. ) ;
#16546 = VERTEX_POINT ( 'NONE', #10756 ) ;
#16547 = SHAPE_REPRESENTATION ( 'Screw 4', ( #5611 ), #14603 ) ;
#16548 = AXIS2_PLACEMENT_3D ( 'NONE', #19757, #14594, #7216 ) ;
#16549 = CARTESIAN_POINT ( 'NONE',  ( 137.4648769445816754, -3661.265785465956469, 2250.004993578675567 ) ) ;
#16550 = ORIENTED_EDGE ( 'NONE', *, *, #21561, .F. ) ;
#16551 = AXIS2_PLACEMENT_3D ( 'NONE', #3760, #1894, #5422 ) ;
#16552 = VERTEX_POINT ( 'NONE', #5842 ) ;
#16553 = VECTOR ( 'NONE', #8995, 1000.000000000000227 ) ;
#16554 = EDGE_CURVE ( 'NONE', #15432, #13716, #1966, .T. ) ;
#16555 = CARTESIAN_POINT ( 'NONE',  ( 50.79999999999999716, -3670.300000000000182, 2260.600000000000364 ) ) ;
#16556 = VERTEX_POINT ( 'NONE', #9347 ) ;
#16557 = DIRECTION ( 'NONE',  ( 0.000000000000000000, 1.000000000000000000, 0.000000000000000000 ) ) ;
#16558 = CARTESIAN_POINT ( 'NONE',  ( 55.57575231171000496, -3694.938000000000102, 2275.001800000000003 ) ) ;
#16559 = EDGE_CURVE ( 'NONE', #8087, #18027, #13933, .T. ) ;
#16560 = ORIENTED_EDGE ( 'NONE', *, *, #6163, .T. ) ;
#16561 = EDGE_CURVE ( 'NONE', #7890, #22920, #16173, .T. ) ;
#16562 = CARTESIAN_POINT ( 'NONE',  ( 7.038650801644599220, -3658.717805898987535, 2244.925821907141199 ) ) ;
#16563 = DIRECTION ( 'NONE',  ( -1.000000000000000000, 0.000000000000000000, 0.000000000000000000 ) ) ;
#16564 = FACE_OUTER_BOUND ( 'NONE', #19942, .T. ) ;
#16565 = AXIS2_PLACEMENT_3D ( 'NONE', #2175, #1819, #16116 ) ;
#16566 = COORDINATED_UNIVERSAL_TIME_OFFSET ( 0, 0, .AHEAD. ) ;
#16567 = FACE_OUTER_BOUND ( 'NONE', #5345, .T. ) ;
#16568 = VECTOR ( 'NONE', #1368, 1000.000000000000000 ) ;
#16569 = VECTOR ( 'NONE', #1428, 1000.000000000000000 ) ;
#16570 = CARTESIAN_POINT ( 'NONE',  ( 142.4905652536138234, -3658.950617808927291, 2249.976257908279877 ) ) ;
#16571 = CARTESIAN_POINT ( 'NONE',  ( 7.837774371996756528, -3662.508315729218339, 2245.815813615873139 ) ) ;
#16572 = ORIENTED_EDGE ( 'NONE', *, *, #7072, .F. ) ;
#16573 = CARTESIAN_POINT ( 'NONE',  ( 142.0316867971999955, -3580.841199999999844, 2242.820000000000164 ) ) ;
#16574 = CARTESIAN_POINT ( 'NONE',  ( 12.70000000000000462, -3596.652698770568804, 2279.817639764978139 ) ) ;
#16575 = DIRECTION ( 'NONE',  ( 0.000000000000000000, 0.000000000000000000, 1.000000000000000000 ) ) ;
#16576 = CIRCLE ( 'NONE', #10220, 1.269999999999882334 ) ;
#16577 = FACE_OUTER_BOUND ( 'NONE', #20413, .T. ) ;
#16578 = CARTESIAN_POINT ( 'NONE',  ( 147.6177065956714785, -3543.413280444305656, 2259.854323493447282 ) ) ;
#16579 = AXIS2_PLACEMENT_3D ( 'NONE', #6516, #2746, #870 ) ;
#16580 = EDGE_LOOP ( 'NONE', ( #6198, #22947, #10132, #10067 ) ) ;
#16581 = CARTESIAN_POINT ( 'NONE',  ( 15.54479972194844528, -3659.504995305038847, 2257.962943247996918 ) ) ;
#16582 = FACE_OUTER_BOUND ( 'NONE', #4870, .T. ) ;
#16583 = CIRCLE ( 'NONE', #18459, 1.269999999999882334 ) ;
#16584 = CARTESIAN_POINT ( 'NONE',  ( 139.6999999999999886, -3570.287499999999909, 2257.592639999999847 ) ) ;
#16585 = ADVANCED_FACE ( 'NONE', ( #21422 ), #93, .T. ) ;
#16586 = EDGE_CURVE ( 'NONE', #15612, #287, #15435, .T. ) ;
#16587 = CLOSED_SHELL ( 'NONE', ( #12434, #15111, #20108, #14480, #7637, #3691, #15687, #9923, #1040, #16719, #8955, #7459 ) ) ;
#16588 = EDGE_CURVE ( 'NONE', #15790, #2161, #12052, .T. ) ;
#16589 = DIRECTION ( 'NONE',  ( 0.000000000000000000, 0.000000000000000000, 1.000000000000000000 ) ) ;
#16590 = CARTESIAN_POINT ( 'NONE',  ( 12.70000000028310616, -3576.362659094871105, 2239.009999999999764 ) ) ;
#16591 = CARTESIAN_POINT ( 'NONE',  ( 95.25000000000000000, -3568.700000000000273, 2250.236800000000130 ) ) ;
#16592 = EDGE_CURVE ( 'NONE', #8560, #8413, #12743, .T. ) ;
#16593 = CARTESIAN_POINT ( 'NONE',  ( 12.69999999997255280, -3636.370159094721657, 2296.591799999999694 ) ) ;
#16594 = ORIENTED_EDGE ( 'NONE', *, *, #4085, .T. ) ;
#16595 = PERSON_AND_ORGANIZATION ( #5446, #1895 ) ;
#16596 = CARTESIAN_POINT ( 'NONE',  ( 145.1168285562762890, -3657.683068618205198, 2245.957879822228278 ) ) ;
#16597 = ADVANCED_FACE ( 'NONE', ( #9118 ), #16904, .T. ) ;
#16598 = CIRCLE ( 'NONE', #18104, 2.844800000000091700 ) ;
#16599 = DIRECTION ( 'NONE',  ( 0.000000000000000000, 0.000000000000000000, 1.000000000000000000 ) ) ;
#16600 = CARTESIAN_POINT ( 'NONE',  ( 20.32000000000000028, -3660.140000000000327, 2247.392000000000280 ) ) ;
#16601 = VERTEX_POINT ( 'NONE', #1849 ) ;
#16602 = ADVANCED_FACE ( 'NONE', ( #14513 ), #12976, .T. ) ;
#16603 = DIRECTION ( 'NONE',  ( 0.000000000000000000, 0.000000000000000000, -1.000000000000000000 ) ) ;
#16604 = EDGE_CURVE ( 'NONE', #19266, #18679, #20131, .T. ) ;
#16605 = CARTESIAN_POINT ( 'NONE',  ( 139.6999999999999886, -3662.197400000000016, 2242.820000000000164 ) ) ;
#16606 = ORIENTED_EDGE ( 'NONE', *, *, #8213, .F. ) ;
#16607 = FACE_OUTER_BOUND ( 'NONE', #13631, .T. ) ;
#16608 = DIRECTION ( 'NONE',  ( 0.000000000000000000, 1.000000000000000000, 0.000000000000000000 ) ) ;
#16609 = EDGE_LOOP ( 'NONE', ( #18160, #14828 ) ) ;
#16610 = DIRECTION ( 'NONE',  ( 0.000000000000000000, 0.000000000000000000, 1.000000000000000000 ) ) ;
#16611 = VECTOR ( 'NONE', #8548, 1000.000000000000000 ) ;
#16612 = CARTESIAN_POINT ( 'NONE',  ( 10.36831320285999958, -3580.841199999999844, 2242.820000000000164 ) ) ;
#16613 = VERTEX_POINT ( 'NONE', #4064 ) ;
#16614 = CARTESIAN_POINT ( 'NONE',  ( 0.000000000000000000, -3660.140000000000327, 2250.998800000000301 ) ) ;
#16615 = CARTESIAN_POINT ( 'NONE',  ( 9.855199999999999960, -3639.502500000000055, 2288.971800000000258 ) ) ;
#16616 = ORIENTED_EDGE ( 'NONE', *, *, #4511, .F. ) ;
#16617 = CARTESIAN_POINT ( 'NONE',  ( 151.4000000000000057, -3695.699999999999818, 2275.001800000000003 ) ) ;
#16618 = VERTEX_POINT ( 'NONE', #21541 ) ;
#16619 = CARTESIAN_POINT ( 'NONE',  ( 145.3787162833025377, -3580.137931053215198, 2244.850299910533977 ) ) ;
#16620 = CALENDAR_DATE ( 2026, 26, 10 ) ;
#16621 = CARTESIAN_POINT ( 'NONE',  ( 17.83565360962044721, -3662.011901429552381, 2245.249457087976225 ) ) ;
#16622 = CIRCLE ( 'NONE', #12520, 5.587999999999926359 ) ;
#16623 = FACE_OUTER_BOUND ( 'NONE', #5015, .T. ) ;
#16624 = CIRCLE ( 'NONE', #20745, 5.460999999999938126 ) ;
#16625 = CARTESIAN_POINT ( 'NONE',  ( 12.60791899384999937, -3576.650200000000041, 2257.592639999999847 ) ) ;
#16626 = AXIS2_PLACEMENT_3D ( 'NONE', #4399, #20339, #8029 ) ;
#16627 = CARTESIAN_POINT ( 'NONE',  ( 142.4730239663999782, -3578.859999866000180, 2250.236800057000437 ) ) ;
#16628 = ORIENTED_EDGE ( 'NONE', *, *, #2824, .F. ) ;
#16629 = ORIENTED_EDGE ( 'NONE', *, *, #6674, .T. ) ;
#16630 = CARTESIAN_POINT ( 'NONE',  ( 10.36831320283682167, -3598.151299999850380, 2296.433984632765714 ) ) ;
#16631 = VERTEX_POINT ( 'NONE', #3712 ) ;
#16632 = CARTESIAN_POINT ( 'NONE',  ( 14.47434230490000040, -3597.266017030000057, 2279.676071933000003 ) ) ;
#16633 = CARTESIAN_POINT ( 'NONE',  ( 142.5447999999993272, -3659.053785370568221, 2256.063560000000962 ) ) ;
#16634 = VERTEX_POINT ( 'NONE', #7362 ) ;
#16635 = LINE ( 'NONE', #11482, #12426 ) ;
#16636 = CIRCLE ( 'NONE', #6554, 5.080000000000000071 ) ;
#16637 = CARTESIAN_POINT ( 'NONE',  ( 1.270000000000000018, -3578.860000000000127, 2247.392000000000280 ) ) ;
#16638 = VECTOR ( 'NONE', #1943, 1000.000000000000000 ) ;
#16639 = ORIENTED_EDGE ( 'NONE', *, *, #16122, .F. ) ;
#16640 = APPLIED_PERSON_AND_ORGANIZATION_ASSIGNMENT ( #604, #14675, ( #10100 ) ) ;
#16641 = AXIS2_PLACEMENT_3D ( 'NONE', #9358, #4080, #1981 ) ;
#16642 = DIRECTION ( 'NONE',  ( 0.000000000000000000, 0.000000000000000000, -1.000000000000000000 ) ) ;
#16643 = CARTESIAN_POINT ( 'NONE',  ( 14.51593956253670825, -3577.305016495025484, 2249.774268863664020 ) ) ;
#16644 =( LENGTH_UNIT ( ) NAMED_UNIT ( * ) SI_UNIT ( .MILLI., .METRE. ) );
#16645 = AXIS2_PLACEMENT_3D ( 'NONE', #4370, #2500, #11284 ) ;
#16646 = DIRECTION ( 'NONE',  ( 0.000000000000000000, 0.000000000000000000, 1.000000000000000000 ) ) ;
#16647 = VERTEX_POINT ( 'NONE', #18355 ) ;
#16648 = LINE ( 'NONE', #14910, #2895 ) ;
#16649 = DATE_TIME_ROLE ( 'classification_date' ) ;
#16650 = EDGE_CURVE ( 'NONE', #13782, #9361, #23154, .T. ) ;
#16651 = DIRECTION ( 'NONE',  ( -1.000000000000000000, 0.000000000000000000, 0.000000000000000000 ) ) ;
#16652 = CYLINDRICAL_SURFACE ( 'NONE', #8697, 2.844799999998995244 ) ;
#16653 = EDGE_LOOP ( 'NONE', ( #1627, #881, #1730, #5707, #16408, #18700, #16427, #21328, #18123, #22139 ) ) ;
#16655 = EDGE_CURVE ( 'NONE', #22767, #2058, #19547, .T. ) ;
#16654 = CARTESIAN_POINT ( 'NONE',  ( -5.588000000000000078, -3544.061999999999898, 2253.487999999999829 ) ) ;
#16656 = ADVANCED_FACE ( 'NONE', ( #19784 ), #16258, .T. ) ;
#16657 = CARTESIAN_POINT ( 'NONE',  ( -12.69999999985358308, -3663.014629489800427, 2247.392000000001190 ) ) ;
#16658 = AXIS2_PLACEMENT_3D ( 'NONE', #13152, #11280, #4470 ) ;
#16659 = ORIENTED_EDGE ( 'NONE', *, *, #16424, .T. ) ;
#16660 = CARTESIAN_POINT ( 'NONE',  ( 140.3462183034946520, -3662.275628691427301, 2249.271390612719188 ) ) ;
#16661 = AXIS2_PLACEMENT_3D ( 'NONE', #8582, #13743, #15728 ) ;
#16662 = EDGE_CURVE ( 'NONE', #4945, #7929, #10867, .T. ) ;
#16663 = ORIENTED_EDGE ( 'NONE', *, *, #15164, .F. ) ;
#16664 = DIRECTION ( 'NONE',  ( -0.8660254037842058938, -0.5000000000004030110, 0.000000000000000000 ) ) ;
#16665 = DIRECTION ( 'NONE',  ( -1.000000000000000000, 0.000000000000000000, 0.000000000000000000 ) ) ;
#16666 = ORIENTED_EDGE ( 'NONE', *, *, #4938, .T. ) ;
#16667 = CARTESIAN_POINT ( 'NONE',  ( 12.69999999999999929, -3659.504999999999654, 2272.030000000000200 ) ) ;
#16668 = DIRECTION ( 'NONE',  ( 1.000000000000000000, 1.224646799147353207E-16, 0.000000000000000000 ) ) ;
#16669 = VERTEX_POINT ( 'NONE', #324 ) ;
#16670 = CARTESIAN_POINT ( 'NONE',  ( 12.69999999999999929, -3659.504999999999654, 2244.978999999999814 ) ) ;
#16671 = DIRECTION ( 'NONE',  ( 0.000000000000000000, 0.000000000000000000, -1.000000000000000000 ) ) ;
#16672 = LINE ( 'NONE', #17130, #12477 ) ;
#16673 = VECTOR ( 'NONE', #15320, 1000.000000000000000 ) ;
#16674 = VECTOR ( 'NONE', #8868, 1000.000000000000000 ) ;
#16675 = CARTESIAN_POINT ( 'NONE',  ( 64.76999999999999602, -3568.700000000000273, 2289.213099999999940 ) ) ;
#16676 = PRODUCT_CONTEXT ( 'NONE', #12767, 'mechanical' ) ;
#16677 = CIRCLE ( 'NONE', #11086, 5.460999999999938126 ) ;
#16678 = ADVANCED_FACE ( 'NONE', ( #10985 ), #1970, .T. ) ;
#16679 = CYLINDRICAL_SURFACE ( 'NONE', #21024, 0.7619999999998753326 ) ;
#16680 =( BOUNDED_CURVE ( )  B_SPLINE_CURVE ( 3, ( #322, #12853, #18239, #5722 ),
 .UNSPECIFIED., .F., .F. ) 
 B_SPLINE_CURVE_WITH_KNOTS ( ( 4, 4 ),
 ( 1.570796327717542518, 3.141592653589902806 ),
 .UNSPECIFIED. ) 
 CURVE ( )  GEOMETRIC_REPRESENTATION_ITEM ( )  RATIONAL_B_SPLINE_CURVE ( ( 1.000000000000000000, 0.8047378543418087782, 0.8047378543418087782, 1.000000000000000000 ) ) 
 REPRESENTATION_ITEM ( '' )  );
#16681 = EDGE_CURVE ( 'NONE', #16201, #20008, #9796, .T. ) ;
#16682 = ADVANCED_FACE ( 'NONE', ( #18587, #15076, #7814 ), #17046, .F. ) ;
#16683 = CARTESIAN_POINT ( 'NONE',  ( 142.3444509448549979, -3658.456267385442970, 2249.685054683717681 ) ) ;
#16684 = CARTESIAN_POINT ( 'NONE',  ( 12.69999999999999929, -3668.712499999999636, 2257.592639999999847 ) ) ;
#16685 = AXIS2_PLACEMENT_3D ( 'NONE', #16765, #599, #13130 ) ;
#16686 = CIRCLE ( 'NONE', #11071, 0.7619999999999294005 ) ;
#16687 = EDGE_LOOP ( 'NONE', ( #22722, #7077, #22628, #7502 ) ) ;
#16688 = DIRECTION ( 'NONE',  ( 0.000000000000000000, 0.000000000000000000, -1.000000000000000000 ) ) ;
#16689 = CIRCLE ( 'NONE', #7358, 7.111999999999785160 ) ;
#16690 = CARTESIAN_POINT ( 'NONE',  ( 12.69999261052944028, -3596.652698770683855, 2279.817639764992691 ) ) ;
#16691 = VERTEX_POINT ( 'NONE', #22431 ) ;
#16692 = AXIS2_PLACEMENT_3D ( 'NONE', #16332, #21493, #9186 ) ;
#16693 = DIRECTION ( 'NONE',  ( 0.000000000000000000, -1.000000000000000000, 0.000000000000000000 ) ) ;
#16694 = PRODUCT_DEFINITION_SHAPE ( 'NONE', 'NONE',  #23175 ) ;
#16695 = AXIS2_PLACEMENT_3D ( 'NONE', #9605, #11470, #16753 ) ;
#16696 = CARTESIAN_POINT ( 'NONE',  ( 18.26004394573143941, -3658.183240515012130, 2245.327057614696514 ) ) ;
#16697 = ORIENTED_EDGE ( 'NONE', *, *, #2199, .F. ) ;
#16698 = ORIENTED_EDGE ( 'NONE', *, *, #11861, .T. ) ;
#16699 = CARTESIAN_POINT ( 'NONE',  ( 147.4602137133928466, -3695.306816721560153, 2260.248793245645629 ) ) ;
#16700 = EDGE_CURVE ( 'NONE', #16884, #22365, #7925, .T. ) ;
#16701 = FACE_OUTER_BOUND ( 'NONE', #17854, .T. ) ;
#16702 = FACE_BOUND ( 'NONE', #17951, .T. ) ;
#16703 = DIRECTION ( 'NONE',  ( 0.000000000000000000, 0.000000000000000000, -1.000000000000000000 ) ) ;
#16704 = DIRECTION ( 'NONE',  ( 1.000000000000000000, 0.000000000000000000, 3.996303350731721563E-14 ) ) ;
#16705 = DIRECTION ( 'NONE',  ( 0.000000000000000000, 0.000000000000000000, -1.000000000000000000 ) ) ;
#16706 = CARTESIAN_POINT ( 'NONE',  ( 7.643488289160662141, -3576.831741762340243, 2245.397138245397400 ) ) ;
#16707 = EDGE_LOOP ( 'NONE', ( #4117, #12418, #2165, #17150, #18957, #13404 ) ) ;
#16708 = DATE_TIME_ROLE ( 'classification_date' ) ;
#16709 = EDGE_CURVE ( 'NONE', #14725, #21716, #14686, .T. ) ;
#16710 = CARTESIAN_POINT ( 'NONE',  ( 145.1202614246111580, -3657.693328148723140, 2245.940466390600250 ) ) ;
#16711 = FACE_OUTER_BOUND ( 'NONE', #14567, .T. ) ;
#16712 = AXIS2_PLACEMENT_3D ( 'NONE', #13860, #21010, #12097 ) ;
#16713 = CYLINDRICAL_SURFACE ( 'NONE', #11598, 2.844800000000001550 ) ;
#16714 = AXIS2_PLACEMENT_3D ( 'NONE', #1384, #17314, #1259 ) ;
#16715 = ORIENTED_EDGE ( 'NONE', *, *, #10653, .F. ) ;
#16716 = AXIS2_PLACEMENT_3D ( 'NONE', #7669, #10959, #18448 ) ;
#16717 = CARTESIAN_POINT ( 'NONE',  ( 134.1072540231934624, -3660.723001229534020, 2244.591060091476265 ) ) ;
#16718 = EDGE_CURVE ( 'NONE', #11610, #6461, #13192, .T. ) ;
#16719 = ADVANCED_FACE ( 'NONE', ( #11433 ), #22205, .F. ) ;
#16720 = AXIS2_PLACEMENT_3D ( 'NONE', #5122, #19409, #10499 ) ;
#16721 = DIRECTION ( 'NONE',  ( 1.000000000000000000, 0.000000000000000000, 0.000000000000000000 ) ) ;
#16722 = EDGE_LOOP ( 'NONE', ( #6831, #9517, #5380, #5817, #4499 ) ) ;
#16723 = B_SPLINE_CURVE_WITH_KNOTS ( 'NONE', 3,
 ( #13180, #16808, #20447, #2629, #9885, #18914 ),
 .UNSPECIFIED., .F., .F.,
 ( 4, 1, 1, 4 ),
 ( 0.000000000000000000, 0.3333333333333000081, 0.6666666666667000474, 1.000000000000000000 ),
 .UNSPECIFIED. ) ;
#16724 = CARTESIAN_POINT ( 'NONE',  ( 13.44550029692929272, -3662.251450944823318, 2249.298748438002804 ) ) ;
#16725 = CARTESIAN_POINT ( 'NONE',  ( 15.54479951278000094, -3579.494996001999880, 2250.165024905999871 ) ) ;
#16726 = ORIENTED_EDGE ( 'NONE', *, *, #8226, .F. ) ;
#16727 = EDGE_CURVE ( 'NONE', #3620, #2616, #1196, .T. ) ;
#16728 = CARTESIAN_POINT ( 'NONE',  ( 12.69999999999999929, -3583.940000000000055, 2262.355140000000119 ) ) ;
#16729 = AXIS2_PLACEMENT_3D ( 'NONE', #10780, #9263, #2228 ) ;
#16730 = CARTESIAN_POINT ( 'NONE',  ( -8.890000000018000392, -3577.513800000000174, 2249.723686796999573 ) ) ;
#16731 = CIRCLE ( 'NONE', #2515, 0.7619999999999294005 ) ;
#16732 = EDGE_LOOP ( 'NONE', ( #10786, #5808, #10210, #21694 ) ) ;
#16733 = DIRECTION ( 'NONE',  ( 0.000000000000000000, 0.000000000000000000, 1.000000000000000000 ) ) ;
#16734 = CARTESIAN_POINT ( 'NONE',  ( 38.10000000000000142, -3644.899999999999636, 2260.600000000000364 ) ) ;
#16735 = EDGE_CURVE ( 'NONE', #3057, #21632, #13311, .T. ) ;
#16736 = ORIENTED_EDGE ( 'NONE', *, *, #9428, .F. ) ;
#16737 = AXIS2_PLACEMENT_3D ( 'NONE', #9571, #18130, #14743 ) ;
#16738 = EDGE_CURVE ( 'NONE', #17590, #19948, #4956, .T. ) ;
#16739 = CIRCLE ( 'NONE', #4760, 0.3809999999999647002 ) ;
#16740 = FACE_OUTER_BOUND ( 'NONE', #17894, .T. ) ;
#16741 = UNCERTAINTY_MEASURE_WITH_UNIT (LENGTH_MEASURE( 1.000000000000000082E-05 ), #21126, 'distance_accuracy_value', 'NONE');
#16742 = EDGE_LOOP ( 'NONE', ( #5106, #9592, #4182, #7973, #15212 ) ) ;
#16743 = DIRECTION ( 'NONE',  ( 0.000000000000000000, 0.000000000000000000, -1.000000000000000000 ) ) ;
#16744 = DATE_TIME_ROLE ( 'classification_date' ) ;
#16745 = DIRECTION ( 'NONE',  ( -1.000000000000000000, 0.000000000000000000, 0.000000000000000000 ) ) ;
#16746 = DIRECTION ( 'NONE',  ( 0.000000000000000000, 0.000000000000000000, -1.000000000000000000 ) ) ;
#16747 = DIRECTION ( 'NONE',  ( 0.000000000000000000, -1.000000000000000000, 0.000000000000000000 ) ) ;
#16748 = CARTESIAN_POINT ( 'NONE',  ( 145.3796772601000100, -3660.139769217999856, 2244.548186305999934 ) ) ;
#16749 = AXIS2_PLACEMENT_3D ( 'NONE', #1253, #22809, #12159 ) ;
#16750 = ADVANCED_FACE ( 'NONE', ( #14961 ), #875, .F. ) ;
#16751 = DIRECTION ( 'NONE',  ( 0.5000000000005969669, -0.8660254037840939834, 0.000000000000000000 ) ) ;
#16752 = VERTEX_POINT ( 'NONE', #7692 ) ;
#16753 = DIRECTION ( 'NONE',  ( -1.000000000000000000, 0.000000000000000000, 0.000000000000000000 ) ) ;
#16754 = VECTOR ( 'NONE', #8135, 1000.000000000000000 ) ;
#16755 = ORIENTED_EDGE ( 'NONE', *, *, #367, .F. ) ;
#16756 = CARTESIAN_POINT ( 'NONE',  ( 9.987313202740898177, -3581.061170452786428, 2239.009999999999764 ) ) ;
#16757 = ORIENTED_EDGE ( 'NONE', *, *, #18178, .F. ) ;
#16758 = LINE ( 'NONE', #16296, #15161 ) ;
#16759 = CARTESIAN_POINT ( 'NONE',  ( 15.39362723101645969, -3543.659322603280998, 2255.389249077201384 ) ) ;
#16760 = EDGE_LOOP ( 'NONE', ( #2048, #21734, #15561, #11167 ) ) ;
#16761 = VERTEX_POINT ( 'NONE', #764 ) ;
#16762 = DIRECTION ( 'NONE',  ( -1.000000000000000000, 0.000000000000000000, 0.000000000000000000 ) ) ;
#16763 = EDGE_LOOP ( 'NONE', ( #11234, #5675, #12785, #12380, #5733, #10591, #21697, #13153, #2222, #11840 ) ) ;
#16764 = CIRCLE ( 'NONE', #16036, 0.7619999999999987894 ) ;
#16765 = CARTESIAN_POINT ( 'NONE',  ( 12.69999999999999929, -3599.497499999999945, 2288.971800000000258 ) ) ;
#16766 = CARTESIAN_POINT ( 'NONE',  ( 14.06012086060861854, -3576.995964396000545, 2249.541211835891318 ) ) ;
#16767 = CARTESIAN_POINT ( 'NONE',  ( 142.1404520028303011, -3580.959877191935448, 2249.315266803219856 ) ) ;
#16768 = ORIENTED_EDGE ( 'NONE', *, *, #15657, .T. ) ;
#16769 = CARTESIAN_POINT ( 'NONE',  ( 35.56000000000000227, -3544.570000000000164, 2244.547199999999975 ) ) ;
#16770 = PERSON_AND_ORGANIZATION_ROLE ( 'design_owner' ) ;
#16771 = CARTESIAN_POINT ( 'NONE',  ( 12.69999999999999929, -3594.036500000000160, 2290.241799999999785 ) ) ;
#16772 = CYLINDRICAL_SURFACE ( 'NONE', #12654, 0.7619999999999294005 ) ;
#16773 = CARTESIAN_POINT ( 'NONE',  ( 136.8551930557000276, -3659.505009668000184, 2250.165028799000083 ) ) ;
#16774 = ORIENTED_EDGE ( 'NONE', *, *, #902, .T. ) ;
#16775 = DIRECTION ( 'NONE',  ( -2.848935406719999894E-12, 1.000000000000000000, 0.000000000000000000 ) ) ;
#16776 = APPROVAL ( #21193, 'UNKNOWN' ) ;
#16777 = ORIENTED_EDGE ( 'NONE', *, *, #16300, .T. ) ;
#16778 = FACE_OUTER_BOUND ( 'NONE', #12356, .T. ) ;
#16779 = DIRECTION ( 'NONE',  ( -1.000000000000000000, 0.000000000000000000, 0.000000000000000000 ) ) ;
#16780 = ADVANCED_FACE ( 'NONE', ( #16711 ), #14856, .F. ) ;
#16781 = ORIENTED_EDGE ( 'NONE', *, *, #20807, .F. ) ;
#16782 = DIRECTION ( 'NONE',  ( 1.000000000000000000, 0.000000000000000000, 0.000000000000000000 ) ) ;
#16783 = PLANE ( 'NONE',  #3176 ) ;
#16784 = VERTEX_POINT ( 'NONE', #2641 ) ;
#16785 = CARTESIAN_POINT ( 'NONE',  ( 7.273601599882602464, -3657.711793654752910, 2245.909852404346566 ) ) ;
#16786 = CARTESIAN_POINT ( 'NONE',  ( 0.7620000000000000107, -3694.938000000000102, 2295.829799999999977 ) ) ;
#16787 = DIRECTION ( 'NONE',  ( 0.000000000000000000, 0.000000000000000000, 1.000000000000000000 ) ) ;
#16788 = LINE ( 'NONE', #11399, #4373 ) ;
#16789 = PERSON_AND_ORGANIZATION ( #5446, #1895 ) ;
#16790 = DIRECTION ( 'NONE',  ( 0.000000000000000000, 1.000000000000000000, 0.000000000000000000 ) ) ;
#16791 = EDGE_LOOP ( 'NONE', ( #13872, #5565, #7143, #22765 ) ) ;
#16792 = AXIS2_PLACEMENT_3D ( 'NONE', #16836, #20149, #890 ) ;
#16794 = CARTESIAN_POINT ( 'NONE',  ( 142.5038613777062437, -3659.021559187911862, 2250.007933345488709 ) ) ;
#16793 = APPLICATION_CONTEXT ( 'configuration controlled 3d designs of mechanical parts and assemblies' ) ;
#16795 = DIRECTION ( 'NONE',  ( 0.000000000000000000, 0.000000000000000000, -1.000000000000000000 ) ) ;
#16796 = ORIENTED_EDGE ( 'NONE', *, *, #3137, .F. ) ;
#16797 = CARTESIAN_POINT ( 'NONE',  ( -12.69999999999999929, -3658.573829546965044, 2244.679313203020683 ) ) ;
#16798 = APPROVAL ( #5224, 'UNSPECIFIED' ) ;
#16799 = CARTESIAN_POINT ( 'NONE',  ( 10.36831320283000046, -3600.843699999999899, 2292.781800000000203 ) ) ;
#16800 = ORIENTED_EDGE ( 'NONE', *, *, #21535, .T. ) ;
#16801 = DIRECTION ( 'NONE',  ( 0.000000000000000000, 0.000000000000000000, -1.000000000000000000 ) ) ;
#16802 = CYLINDRICAL_SURFACE ( 'NONE', #17817, 0.3809999999999993947 ) ;
#16803 = EDGE_CURVE ( 'NONE', #18833, #22793, #20563, .T. ) ;
#16804 = ORIENTED_EDGE ( 'NONE', *, *, #8644, .F. ) ;
#16805 = ORIENTED_EDGE ( 'NONE', *, *, #15305, .T. ) ;
#16806 = CARTESIAN_POINT ( 'NONE',  ( -8.890000000047999507, -3658.793800000000374, 2245.060313203000078 ) ) ;
#16807 = EDGE_CURVE ( 'NONE', #7313, #8026, #18499, .T. ) ;
#16808 = CARTESIAN_POINT ( 'NONE',  ( 20.31206600734000034, -3694.758336080999925, 2260.533847755999886 ) ) ;
#16809 = AXIS2_PLACEMENT_3D ( 'NONE', #7806, #2632, #13073 ) ;
#16810 = DIRECTION ( 'NONE',  ( 0.000000000000000000, 0.000000000000000000, -1.000000000000000000 ) ) ;
#16811 = EDGE_CURVE ( 'NONE', #11524, #5223, #2335, .T. ) ;
#16812 = DIRECTION ( 'NONE',  ( -1.000000000000000000, 0.000000000000000000, -1.295098308109999907E-13 ) ) ;
#16813 = FACE_OUTER_BOUND ( 'NONE', #11053, .T. ) ;
#16814 = CARTESIAN_POINT ( 'NONE',  ( 8.037678690397633829, -3576.188730137088442, 2246.379736642491480 ) ) ;
#16815 = ORIENTED_EDGE ( 'NONE', *, *, #17665, .T. ) ;
#16816 = APPROVAL_DATE_TIME ( #9678, #17514 ) ;
#16817 = CARTESIAN_POINT ( 'NONE',  ( 105.2067999999999870, -3670.300000000000182, 2239.771999999999935 ) ) ;
#16818 = CARTESIAN_POINT ( 'NONE',  ( 12.70000000000000107, -3590.289999999999964, 2279.817639999999756 ) ) ;
#16819 = CARTESIAN_POINT ( 'NONE',  ( 9.926995637850000165, -3660.140002548000211, 2250.236801297000056 ) ) ;
#16820 = LOCAL_TIME ( 17, 37, 43.00000000000000000, #20867 ) ;
#16821 = EDGE_CURVE ( 'NONE', #20008, #16201, #18057, .T. ) ;
#16822 = CIRCLE ( 'NONE', #8976, 6.477000000000000313 ) ;
#16823 = ORIENTED_EDGE ( 'NONE', *, *, #2676, .F. ) ;
#16824 = CARTESIAN_POINT ( 'NONE',  ( 134.0525542150678291, -3660.427269758552029, 2244.547227117760031 ) ) ;
#16825 = DIRECTION ( 'NONE',  ( 1.000000000000000000, 0.000000000000000000, 0.000000000000000000 ) ) ;
#16826 = CARTESIAN_POINT ( 'NONE',  ( 134.5329181263396094, -3577.053440065938503, 2245.194077375531833 ) ) ;
#16827 = ORIENTED_EDGE ( 'NONE', *, *, #15747, .F. ) ;
#16828 = DIRECTION ( 'NONE',  ( 0.000000000000000000, -1.000000000000000000, 0.000000000000000000 ) ) ;
#16829 = FACE_OUTER_BOUND ( 'NONE', #13654, .T. ) ;
#16830 = CARTESIAN_POINT ( 'NONE',  ( 95.25000000000000000, -3543.300000000000182, 2251.506800000000112 ) ) ;
#16831 = ORIENTED_EDGE ( 'NONE', *, *, #5991, .F. ) ;
#16832 = DIRECTION ( 'NONE',  ( -1.000000000000000000, 3.885294924331999768E-13, 2.590196616220999964E-13 ) ) ;
#16833 = DIRECTION ( 'NONE',  ( 0.000000000000000000, -1.000000000000000000, 0.000000000000000000 ) ) ;
#16834 = AXIS2_PLACEMENT_3D ( 'NONE', #17079, #4660, #4897 ) ;
#16835 = EDGE_CURVE ( 'NONE', #22295, #4559, #7956, .T. ) ;
#16836 = CARTESIAN_POINT ( 'NONE',  ( 139.6999999999999886, -3579.494999999999891, 2244.978999999999814 ) ) ;
#16837 = DIRECTION ( 'NONE',  ( -1.000000000000000000, 0.000000000000000000, 0.000000000000000000 ) ) ;
#16838 = APPLIED_APPROVAL_ASSIGNMENT ( #10617, ( #6021 ) ) ;
#16839 = VERTEX_POINT ( 'NONE', #21046 ) ;
#16840 = EDGE_CURVE ( 'NONE', #16546, #19496, #22155, .T. ) ;
#16841 = EDGE_CURVE ( 'NONE', #15348, #19268, #21629, .T. ) ;
#16842 = CIRCLE ( 'NONE', #6762, 2.844799999998897988 ) ;
#16843 = CARTESIAN_POINT ( 'NONE',  ( 137.3683132029982517, -3658.158799999858729, 2239.391000000000076 ) ) ;
#16844 = EDGE_LOOP ( 'NONE', ( #11469, #13173, #21238, #8553 ) ) ;
#16845 = CARTESIAN_POINT ( 'NONE',  ( 145.3744937373275832, -3580.174051493410389, 2244.868862703849118 ) ) ;
#16846 = CONTEXT_DEPENDENT_SHAPE_REPRESENTATION ( #11690, #14837 ) ;
#16847 = CARTESIAN_POINT ( 'NONE',  ( 145.3976541156836788, -3579.044846244369637, 2244.552343491880492 ) ) ;
#16848 = CARTESIAN_POINT ( 'NONE',  ( 17.56682579340610673, -3662.500841285317165, 2245.804760078034178 ) ) ;
#16849 = CIRCLE ( 'NONE', #760, 0.7619999999999987894 ) ;
#16850 = DIRECTION ( 'NONE',  ( 0.000000000000000000, 1.000000000000000000, 0.000000000000000000 ) ) ;
#16851 = CARTESIAN_POINT ( 'NONE',  ( 151.1299999999999955, -3544.570000000000164, 2240.279999999999745 ) ) ;
#16852 = SECURITY_CLASSIFICATION ( '', '', #6899 ) ;
#16853 = CARTESIAN_POINT ( 'NONE',  ( 116.8400000000000034, -3544.570000000000164, 2247.392000000000280 ) ) ;
#16854 = ORIENTED_EDGE ( 'NONE', *, *, #15519, .T. ) ;
#16855 = APPROVAL_PERSON_ORGANIZATION ( #21760, #12657, #2198 ) ;
#16856 = ADVANCED_FACE ( 'NONE', ( #3456 ), #21735, .T. ) ;
#16857 = DIRECTION ( 'NONE',  ( 0.000000000000000000, 0.000000000000000000, -1.000000000000000000 ) ) ;
#16858 = AXIS2_PLACEMENT_3D ( 'NONE', #19653, #15910, #13718 ) ;
#16859 = CARTESIAN_POINT ( 'NONE',  ( 142.4126867972000241, -3657.938829547000296, 2239.009999999999764 ) ) ;
#16860 = ORIENTED_EDGE ( 'NONE', *, *, #5980, .T. ) ;
#16861 = CARTESIAN_POINT ( 'NONE',  ( 20.32000000000000028, -3543.299999999999727, 2285.606299999999919 ) ) ;
#16862 = CARTESIAN_POINT ( 'NONE',  ( 142.3973403518663758, -3660.427758120067665, 2257.924723938623174 ) ) ;
#16863 = VERTEX_POINT ( 'NONE', #10727 ) ;
#16864 = AXIS2_PLACEMENT_3D ( 'NONE', #16917, #862, #8028 ) ;
#16865 = ORIENTED_EDGE ( 'NONE', *, *, #18597, .F. ) ;
#16866 = ORIENTED_EDGE ( 'NONE', *, *, #22160, .F. ) ;
#16867 = CARTESIAN_POINT ( 'NONE',  ( 19.05000000000000071, -3662.045000000000073, 2247.392000000000280 ) ) ;
#16868 = ORIENTED_EDGE ( 'NONE', *, *, #12096, .T. ) ;
#16869 = DIRECTION ( 'NONE',  ( -1.000000000000000000, 0.000000000000000000, 0.000000000000000000 ) ) ;
#16870 = EDGE_CURVE ( 'NONE', #22886, #18714, #20303, .T. ) ;
#16871 = CARTESIAN_POINT ( 'NONE',  ( 11.90373727042107355, -3576.763824424820086, 2249.315280365585750 ) ) ;
#16872 =( NAMED_UNIT ( * ) SI_UNIT ( $, .STERADIAN. ) SOLID_ANGLE_UNIT ( ) );
#16873 = CARTESIAN_POINT ( 'NONE',  ( 142.4777174751457380, -3580.110796106637736, 2249.947098715658285 ) ) ;
#16874 = ORIENTED_EDGE ( 'NONE', *, *, #18110, .T. ) ;
#16875 = CARTESIAN_POINT ( 'NONE',  ( 0.7620000000000000107, -3694.938000000000102, 2295.829799999999977 ) ) ;
#16876 = COORDINATED_UNIVERSAL_TIME_OFFSET ( 0, 0, .AHEAD. ) ;
#16877 = CARTESIAN_POINT ( 'NONE',  ( 3.048000000000000043, -3694.938000000000102, 2238.248000000000047 ) ) ;
#16878 = FACE_BOUND ( 'NONE', #15811, .T. ) ;
#16879 = PERSON ( 'NAUO-PER2', 'UNSPECIFIED', 'UNSPECIFIED', ('UNSPECIFIED'), ('UNSPECIFIED'), ('UNSPECIFIED') ) ;
#16880 = CIRCLE ( 'NONE', #21396, 0.7619999999999294005 ) ;
#16881 = PRODUCT ( 'Base Plate', 'Base Plate', '', ( #7841 ) ) ;
#16882 = FACE_OUTER_BOUND ( 'NONE', #4652, .T. ) ;
#16883 = CIRCLE ( 'NONE', #17262, 3.606799999999993567 ) ;
#16884 = VERTEX_POINT ( 'NONE', #14486 ) ;
#16885 = EDGE_CURVE ( 'NONE', #9004, #4163, #2688, .T. ) ;
#16886 = DIRECTION ( 'NONE',  ( -1.000000000000000000, -2.848935406719999894E-12, 0.000000000000000000 ) ) ;
#16887 = EDGE_CURVE ( 'NONE', #20367, #5163, #12433, .T. ) ;
#16888 = EDGE_LOOP ( 'NONE', ( #114, #11137, #4274, #13044 ) ) ;
#16889 = VERTEX_POINT ( 'NONE', #3572 ) ;
#16890 = DIRECTION ( 'NONE',  ( 0.000000000000000000, -1.000000000000000000, 0.000000000000000000 ) ) ;
#16891 = ORIENTED_EDGE ( 'NONE', *, *, #18884, .F. ) ;
#16892 = LINE ( 'NONE', #8228, #12040 ) ;
#16893 = DIRECTION ( 'NONE',  ( 0.000000000000000000, 0.000000000000000000, -1.000000000000000000 ) ) ;
#16894 = AXIS2_PLACEMENT_3D ( 'NONE', #16902, #9756, #11622 ) ;
#16895 = ORIENTED_EDGE ( 'NONE', *, *, #21406, .F. ) ;
#16896 = CIRCLE ( 'NONE', #21781, 0.7619999999999294005 ) ;
#16897 = DIRECTION ( 'NONE',  ( -1.224646799147353207E-16, 1.000000000000000000, 0.000000000000000000 ) ) ;
#16898 = SHAPE_REPRESENTATION_RELATIONSHIP ( 'NONE' , 'NONE' ,  #7730, #21380 ) ;
#16899 = FACE_OUTER_BOUND ( 'NONE', #19702, .T. ) ;
#16900 = CARTESIAN_POINT ( 'NONE',  ( 9.987313202864001482, -3661.071170452999922, 2239.009999999999764 ) ) ;
#16901 = PERSON_AND_ORGANIZATION_ROLE ( 'creator' ) ;
#16902 = CARTESIAN_POINT ( 'NONE',  ( 76.20000000000000284, -3568.700000000000273, 2261.869999999999891 ) ) ;
#16903 = FACE_OUTER_BOUND ( 'NONE', #20027, .T. ) ;
#16904 = TOROIDAL_SURFACE ( 'NONE', #811, 1.905000000000000027, 1.270000000000000018 ) ;
#16905 = CARTESIAN_POINT ( 'NONE',  ( 12.69999999999999929, -3653.027999999999793, 2262.355140000000119 ) ) ;
#16906 = DIRECTION ( 'NONE',  ( 5.432398939370942693E-28, 1.000000000000000000, 2.336881798971000105E-14 ) ) ;
#16907 = VECTOR ( 'NONE', #787, 1000.000000000000000 ) ;
#16908 = B_SPLINE_CURVE_WITH_KNOTS ( 'NONE', 3,
 ( #10400, #19075, #8540, #15562 ),
 .UNSPECIFIED., .F., .F.,
 ( 4, 4 ),
 ( 0.000000000000000000, 5.006989800018624494E-06 ),
 .UNSPECIFIED. ) ;
#16909 = EDGE_LOOP ( 'NONE', ( #1754, #11099, #20732, #13093 ) ) ;
#16910 = VECTOR ( 'NONE', #19485, 1000.000000000000000 ) ;
#16911 = AXIS2_PLACEMENT_3D ( 'NONE', #22222, #9588, #22005 ) ;
#16912 = ORIENTED_EDGE ( 'NONE', *, *, #9941, .T. ) ;
#16913 = DIRECTION ( 'NONE',  ( -0.5000000000005969669, -0.8660254037840939834, 0.000000000000000000 ) ) ;
#16914 = DIRECTION ( 'NONE',  ( -1.224646799147353207E-16, 1.000000000000000000, 0.000000000000000000 ) ) ;
#16915 = ORIENTED_EDGE ( 'NONE', *, *, #10850, .F. ) ;
#16916 = ORIENTED_EDGE ( 'NONE', *, *, #17738, .T. ) ;
#16917 = CARTESIAN_POINT ( 'NONE',  ( 136.2852881834000129, -3544.570000000000164, 2254.853250718999789 ) ) ;
#16918 = CARTESIAN_POINT ( 'NONE',  ( 64.76999999999999602, -3670.300000000000182, 2289.213099999999940 ) ) ;
#16919 = AXIS2_PLACEMENT_3D ( 'NONE', #16289, #10433, #14543 ) ;
#16920 = CARTESIAN_POINT ( 'NONE',  ( 12.59469521408999881, -3602.342298742000366, 2279.817638609000369 ) ) ;
#16921 = DIRECTION ( 'NONE',  ( 1.000000000000000000, 0.000000000000000000, 0.000000000000000000 ) ) ;
#16922 = CARTESIAN_POINT ( 'NONE',  ( 142.4431999999993366, -3578.616742952568075, 2255.967040000000907 ) ) ;
#16923 = CIRCLE ( 'NONE', #19941, 2.844799999999999773 ) ;
#16924 = CARTESIAN_POINT ( 'NONE',  ( 20.53015091878355491, -3695.459526430383903, 2260.073662062739913 ) ) ;
#16925 = ORIENTED_EDGE ( 'NONE', *, *, #8673, .F. ) ;
#16926 = DATE_TIME_ROLE ( 'creation_date' ) ;
#16927 = APPLIED_PERSON_AND_ORGANIZATION_ASSIGNMENT ( #15998, #16343, ( #20962 ) ) ;
#16928 = AXIS2_PLACEMENT_3D ( 'NONE', #12329, #8817, #10215 ) ;
#16929 = ADVANCED_FACE ( 'NONE', ( #8858 ), #1936, .T. ) ;
#16930 = CARTESIAN_POINT ( 'NONE',  ( 12.69999999999999929, -3655.060000000000400, 2268.705139999999574 ) ) ;
#16931 = DIRECTION ( 'NONE',  ( -1.000000000000000000, 0.000000000000000000, 0.000000000000000000 ) ) ;
#16932 = ADVANCED_FACE ( 'NONE', ( #5583 ), #5710, .T. ) ;
#16933 = CARTESIAN_POINT ( 'NONE',  ( 16.19063073439513190, -3543.299999999999727, 2282.113800000000083 ) ) ;
#16934 = EDGE_CURVE ( 'NONE', #8091, #2574, #21055, .T. ) ;
#16935 = ORIENTED_EDGE ( 'NONE', *, *, #6674, .F. ) ;
#16936 = CIRCLE ( 'NONE', #21826, 0.7619999999999294005 ) ;
#16937 = CARTESIAN_POINT ( 'NONE',  ( 25.39999999999999858, -3568.700000000000273, 2239.009999999999764 ) ) ;
#16938 = EDGE_CURVE ( 'NONE', #16647, #10320, #7937, .T. ) ;
#16939 = CARTESIAN_POINT ( 'NONE',  ( 12.70000000002640839, -3656.812599999929262, 2239.391000000000076 ) ) ;
#16940 = CARTESIAN_POINT ( 'NONE',  ( 134.1465012860365675, -3578.137695944618372, 2244.636253112222221 ) ) ;
#16941 = ORIENTED_EDGE ( 'NONE', *, *, #20590, .T. ) ;
#16942 = AXIS2_PLACEMENT_3D ( 'NONE', #19249, #6951, #3184 ) ;
#16943 = CARTESIAN_POINT ( 'NONE',  ( 79.80679999999999552, -3670.300000000000182, 2260.600000000000364 ) ) ;
#16944 = DIRECTION ( 'NONE',  ( -1.000000000000000000, 2.330758767201999921E-14, 2.343004830739999973E-14 ) ) ;
#16945 = AXIS2_PLACEMENT_3D ( 'NONE', #11855, #2947, #6822 ) ;
#16946 = LINE ( 'NONE', #17762, #21192 ) ;
#16947 = ORIENTED_EDGE ( 'NONE', *, *, #11771, .F. ) ;
#16948 = EDGE_CURVE ( 'NONE', #15032, #7066, #14365, .T. ) ;
#16949 = CARTESIAN_POINT ( 'NONE',  ( 1.270000000000000018, -3544.570000000000164, 2259.329999999999927 ) ) ;
#16950 =( BOUNDED_CURVE ( )  B_SPLINE_CURVE ( 3, ( #21291, #7223, #10845, #21402 ),
 .UNSPECIFIED., .F., .T. ) 
 B_SPLINE_CURVE_WITH_KNOTS ( ( 4, 4 ),
 ( 1.570796326968375789, 3.141592653589766471 ),
 .UNSPECIFIED. ) 
 CURVE ( )  GEOMETRIC_REPRESENTATION_ITEM ( )  RATIONAL_B_SPLINE_CURVE ( ( 1.000000000000000000, 0.8047378541652607797, 0.8047378541652607797, 1.000000000000000000 ) ) 
 REPRESENTATION_ITEM ( '' )  );
#16951 = CARTESIAN_POINT ( 'NONE',  ( 12.69999999999999929, -3659.504999999999654, 2245.359999999999673 ) ) ;
#16952 = DIRECTION ( 'NONE',  ( -1.000000000000000000, 0.000000000000000000, 0.000000000000000000 ) ) ;
#16953 = CARTESIAN_POINT ( 'NONE',  ( 76.20000000000000284, -3568.700000000000273, 2260.600000000000364 ) ) ;
#16954 = EDGE_CURVE ( 'NONE', #20566, #18833, #21511, .T. ) ;
#16955 = ORIENTED_EDGE ( 'NONE', *, *, #7098, .T. ) ;
#16956 = CIRCLE ( 'NONE', #6876, 3.606800000000000228 ) ;
#16957 = ORIENTED_EDGE ( 'NONE', *, *, #15817, .F. ) ;
#16958 = CARTESIAN_POINT ( 'NONE',  ( 136.8552000000009912, -3579.494999999999891, 2272.030000000000200 ) ) ;
#16959 = ORIENTED_EDGE ( 'NONE', *, *, #11778, .F. ) ;
#16960 = CARTESIAN_POINT ( 'NONE',  ( 142.5447999999990998, -3659.316313936683400, 2257.962944264954331 ) ) ;
#16961 = PERSON_AND_ORGANIZATION_ROLE ( 'classification_officer' ) ;
#16962 = CLOSED_SHELL ( 'NONE', ( #16968, #10228, #11009, #4329, #255, #13757, #14186, #18686, #3539, #19041, #254, #8489, #9795, #13546, #11850, #13576, #16682, #3410, #18661, #17852, #23051, #7632, #15224, #11356, #18750, #2202, #1325, #11422, #2511, #8846, #15385, #11832, #21041, #20414, #19896, #355, #11949, #21621, #14882, #15976, #1261, #18586, #6374, #8948, #661, #21196, #116, #20707, #15308, #8218, #18324, #19167, #4994, #942, #13635, #17595, #9531, #851, #13672, #21833, #5165, #14170, #3716, #13391, #10552, #6750, #18446, #19091, #17225, #10726, #15891, #11363, #12930, #3120, #6213, #18615, #6884, #22549, #16160 ) ) ;
#16963 = DIRECTION ( 'NONE',  ( 0.000000000000000000, 0.000000000000000000, -1.000000000000000000 ) ) ;
#16964 = CARTESIAN_POINT ( 'NONE',  ( 17.93858170739038371, -3661.789460736868023, 2245.074020119504439 ) ) ;
#16965 = EDGE_CURVE ( 'NONE', #20602, #2972, #12805, .T. ) ;
#16966 = ADVANCED_FACE ( 'NONE', ( #12484 ), #11661, .T. ) ;
#16967 = CARTESIAN_POINT ( 'NONE',  ( 137.1599999999999966, -3660.786127253999894, 2255.774000000000342 ) ) ;
#16968 = ADVANCED_FACE ( 'NONE', ( #7551 ), #460, .T. ) ;
#16969 = DIRECTION ( 'NONE',  ( 0.8660254037825932949, 0.5000000000031962211, 0.000000000000000000 ) ) ;
#16970 = CARTESIAN_POINT ( 'NONE',  ( 136.9932263412491693, -3578.570683720540728, 2250.236800207163924 ) ) ;
#16971 = ORIENTED_EDGE ( 'NONE', *, *, #13966, .T. ) ;
#16972 = AXIS2_PLACEMENT_3D ( 'NONE', #15716, #19577, #5177 ) ;
#16973 = DIRECTION ( 'NONE',  ( -2.330758767202000237E-14, -1.000000000000000000, -1.224646799141892318E-16 ) ) ;
#16974 = LINE ( 'NONE', #2570, #18534 ) ;
#16975 = ORIENTED_EDGE ( 'NONE', *, *, #6706, .F. ) ;
#16976 = LINE ( 'NONE', #6447, #15530 ) ;
#16977 = CARTESIAN_POINT ( 'NONE',  ( 141.5805787459278804, -3661.647520101402733, 2257.752117344049111 ) ) ;
#16978 = VERTEX_POINT ( 'NONE', #12606 ) ;
#16979 = EDGE_LOOP ( 'NONE', ( #4853, #14337, #7191, #1179 ) ) ;
#16980 = ORIENTED_EDGE ( 'NONE', *, *, #12705, .T. ) ;
#16981 = DIRECTION ( 'NONE',  ( -0.000000000000000000, 1.224646799147353207E-16, 1.000000000000000000 ) ) ;
#16982 = ORIENTED_EDGE ( 'NONE', *, *, #21318, .T. ) ;
#16983 = DIRECTION ( 'NONE',  ( 1.000000000000000000, 0.000000000000000000, 0.000000000000000000 ) ) ;
#16984 = CARTESIAN_POINT ( 'NONE',  ( 11.61431908031736171, -3576.865156646217201, 2249.420288324090507 ) ) ;
#16985 = CARTESIAN_POINT ( 'NONE',  ( 141.8090081642606322, -3581.404182753561145, 2248.664805393861116 ) ) ;
#16986 = ORIENTED_EDGE ( 'NONE', *, *, #6648, .T. ) ;
#16987 = DIRECTION ( 'NONE',  ( -1.000000000000000000, 0.000000000000000000, 0.000000000000000000 ) ) ;
#16988 = CIRCLE ( 'NONE', #18848, 0.7619999999999294005 ) ;
#16989 = PERSON_AND_ORGANIZATION ( #5446, #1895 ) ;
#16990 = CIRCLE ( 'NONE', #12524, 3.175000000000149925 ) ;
#16991 = DIRECTION ( 'NONE',  ( 1.224646799141920914E-16, -1.000000000000000000, -2.336881798971000421E-14 ) ) ;
#16992 = DIRECTION ( 'NONE',  ( 1.000000000000000000, 0.000000000000000000, 0.000000000000000000 ) ) ;
#16993 = CARTESIAN_POINT ( 'NONE',  ( 134.2595036476987502, -3657.754874278681200, 2245.841254873516846 ) ) ;
#16994 = VERTEX_POINT ( 'NONE', #66 ) ;
#16995 = CARTESIAN_POINT ( 'NONE',  ( 12.69999999999999929, -3641.407499999999800, 2263.571799999999712 ) ) ;
#16996 = EDGE_CURVE ( 'NONE', #20246, #10320, #8708, .T. ) ;
#16997 = EDGE_CURVE ( 'NONE', #8573, #7121, #19513, .T. ) ;
#16998 = ORIENTED_EDGE ( 'NONE', *, *, #16588, .F. ) ;
#16999 = EDGE_CURVE ( 'NONE', #10638, #22029, #7582, .T. ) ;
#17000 = B_SPLINE_CURVE_WITH_KNOTS ( 'NONE', 3,
 ( #14153, #12032, #19414, #19303 ),
 .UNSPECIFIED., .F., .F.,
 ( 4, 4 ),
 ( 0.000000000000000000, 1.000000000000000000 ),
 .UNSPECIFIED. ) ;
#17001 = EDGE_LOOP ( 'NONE', ( #3373, #22849 ) ) ;
#17002 = AXIS2_PLACEMENT_3D ( 'NONE', #17758, #3344, #20816 ) ;
#17003 = AXIS2_PLACEMENT_3D ( 'NONE', #11528, #745, #9545 ) ;
#17004 = CARTESIAN_POINT ( 'NONE',  ( 7.619999999999999218, -3579.494999999999891, 2239.009999999999764 ) ) ;
#17005 = VECTOR ( 'NONE', #7539, 1000.000000000000000 ) ;
#17006 = VERTEX_POINT ( 'NONE', #18780 ) ;
#17007 = VERTEX_POINT ( 'NONE', #11520 ) ;
#17008 = DIRECTION ( 'NONE',  ( 1.163002179514000079E-14, 1.000000000000000000, 7.088775189419001325E-13 ) ) ;
#17009 = DIRECTION ( 'NONE',  ( 1.000000000000000000, 0.000000000000000000, 0.000000000000000000 ) ) ;
#17010 = EDGE_CURVE ( 'NONE', #7174, #1860, #14704, .T. ) ;
#17011 = ORIENTED_EDGE ( 'NONE', *, *, #12458, .T. ) ;
#17012 = CARTESIAN_POINT ( 'NONE',  ( 7.172952441013247693, -3658.051458389673371, 2245.460178138798256 ) ) ;
#17013 =( LENGTH_UNIT ( ) NAMED_UNIT ( * ) SI_UNIT ( .MILLI., .METRE. ) );
#17014 = CARTESIAN_POINT ( 'NONE',  ( 139.6999999999999886, -3579.494999999999891, 2245.359999999999673 ) ) ;
#17015 = DIRECTION ( 'NONE',  ( 1.000000000000000000, 0.000000000000000000, 0.000000000000000000 ) ) ;
#17016 = EDGE_CURVE ( 'NONE', #17151, #7277, #9461, .T. ) ;
#17017 = DATE_AND_TIME ( #20770, #7105 ) ;
#17018 = EDGE_CURVE ( 'NONE', #22138, #13513, #20538, .T. ) ;
#17019 = CARTESIAN_POINT ( 'NONE',  ( 7.619999999999999218, -3579.494999999999891, 2244.978999999999814 ) ) ;
#17020 = CARTESIAN_POINT ( 'NONE',  ( 9.209369265563442042, -3543.299999999999727, 2282.113800000095125 ) ) ;
#17021 = AXIS2_PLACEMENT_3D ( 'NONE', #16799, #15484, #2944 ) ;
#17022 = DIRECTION ( 'NONE',  ( 0.000000000000000000, 0.000000000000000000, 1.000000000000000000 ) ) ;
#17023 = CARTESIAN_POINT ( 'NONE',  ( 12.69999999999999929, -3590.289999999999964, 2268.705139999999574 ) ) ;
#17024 = ORIENTED_EDGE ( 'NONE', *, *, #21610, .T. ) ;
#17025 = DIRECTION ( 'NONE',  ( 0.000000000000000000, 0.000000000000000000, 1.000000000000000000 ) ) ;
#17026 = EDGE_CURVE ( 'NONE', #13045, #14116, #20320, .T. ) ;
#17027 = ORIENTED_EDGE ( 'NONE', *, *, #7798, .T. ) ;
#17028 = EDGE_LOOP ( 'NONE', ( #16982, #14922, #11044, #2539, #18429 ) ) ;
#17029 = FACE_OUTER_BOUND ( 'NONE', #10565, .T. ) ;
#17030 = CARTESIAN_POINT ( 'NONE',  ( 18.30933195705248195, -3658.407053146634553, 2245.132319941641526 ) ) ;
#17031 = VERTEX_POINT ( 'NONE', #7787 ) ;
#17032 = EDGE_LOOP ( 'NONE', ( #18032, #5092, #8222, #1626 ) ) ;
#17033 = CARTESIAN_POINT ( 'NONE',  ( 139.7000000002929596, -3576.362659094888386, 2239.009999999999764 ) ) ;
#17034 = CARTESIAN_POINT ( 'NONE',  ( 18.40320150486666506, -3579.070516913197025, 2244.547180105589632 ) ) ;
#17035 = AXIS2_PLACEMENT_3D ( 'NONE', #19439, #12408, #21209 ) ;
#17036 = CARTESIAN_POINT ( 'NONE',  ( 0.7620000000000000107, -3544.061999999999898, 2239.771999999999935 ) ) ;
#17037 = DIRECTION ( 'NONE',  ( -1.000000000000000000, 0.000000000000000000, 0.000000000000000000 ) ) ;
#17038 = AXIS2_PLACEMENT_3D ( 'NONE', #18623, #2569, #798 ) ;
#17039 = LINE ( 'NONE', #11536, #15450 ) ;
#17040 = DIRECTION ( 'NONE',  ( 0.000000000000000000, 0.000000000000000000, 1.000000000000000000 ) ) ;
#17041 = CARTESIAN_POINT ( 'NONE',  ( 15.03168679706394428, -3598.151299999898129, 2296.210799999999836 ) ) ;
#17042 = VERTEX_POINT ( 'NONE', #15279 ) ;
#17043 = APPROVAL_ROLE ( '' ) ;
#17044 = VERTEX_POINT ( 'NONE', #16905 ) ;
#17045 = CARTESIAN_POINT ( 'NONE',  ( 145.3463507443650258, -3658.589118495387083, 2244.993626476412828 ) ) ;
#17046 = PLANE ( 'NONE',  #3077 ) ;
#17047 = CARTESIAN_POINT ( 'NONE',  ( 57.14999999999999858, -3543.299999999999727, 2247.392000000000280 ) ) ;
#17048 = VECTOR ( 'NONE', #22310, 1000.000000000000000 ) ;
#17049 = ORIENTED_EDGE ( 'NONE', *, *, #10437, .F. ) ;
#17050 = VECTOR ( 'NONE', #21520, 1000.000000000000000 ) ;
#17051 = CIRCLE ( 'NONE', #5863, 3.606799999999001027 ) ;
#17052 = DIRECTION ( 'NONE',  ( 0.000000000000000000, 1.000000000000000000, 0.000000000000000000 ) ) ;
#17053 = CARTESIAN_POINT ( 'NONE',  ( 144.5560466049839192, -3662.518293485689810, 2245.831027411331434 ) ) ;
#17054 = EDGE_LOOP ( 'NONE', ( #13218, #12119, #21109, #20060 ) ) ;
#17055 = DIRECTION ( 'NONE',  ( -1.000000000000000000, 0.000000000000000000, 0.000000000000000000 ) ) ;
#17056 = AXIS2_PLACEMENT_3D ( 'NONE', #11190, #18105, #19992 ) ;
#17057 = CARTESIAN_POINT ( 'NONE',  ( 14.29440584201453568, -3661.861461941862672, 2249.657208667620580 ) ) ;
#17058 = APPLIED_PERSON_AND_ORGANIZATION_ASSIGNMENT ( #8567, #23071, ( #22928 ) ) ;
#17059 = LINE ( 'NONE', #2766, #15194 ) ;
#17060 = CIRCLE ( 'NONE', #6232, 5.715000000000999947 ) ;
#17061 = ORIENTED_EDGE ( 'NONE', *, *, #18385, .F. ) ;
#17062 = CARTESIAN_POINT ( 'NONE',  ( 142.7460459831000037, -3581.600847922473804, 2246.630002817673358 ) ) ;
#17063 = CARTESIAN_POINT ( 'NONE',  ( 13.63269713621999912, -3636.808664902999681, 2279.779803621000156 ) ) ;
#17064 = EDGE_CURVE ( 'NONE', #15650, #12135, #9759, .T. ) ;
#17065 = DIRECTION ( 'NONE',  ( 0.000000000000000000, 0.000000000000000000, -1.000000000000000000 ) ) ;
#17066 = FACE_OUTER_BOUND ( 'NONE', #6990, .T. ) ;
#17067 = CYLINDRICAL_SURFACE ( 'NONE', #9088, 2.844799999998998796 ) ;
#17068 = ORIENTED_EDGE ( 'NONE', *, *, #11128, .F. ) ;
#17069 = VERTEX_POINT ( 'NONE', #8017 ) ;
#17070 = EDGE_CURVE ( 'NONE', #5647, #3812, #9096, .T. ) ;
#17071 = CIRCLE ( 'NONE', #611, 5.460999999999938126 ) ;
#17072 = LINE ( 'NONE', #2779, #19166 ) ;
#17073 = VERTEX_POINT ( 'NONE', #2284 ) ;
#17074 = CARTESIAN_POINT ( 'NONE',  ( 140.4431196388952401, -3656.752565539492480, 2257.615983594234422 ) ) ;
#17075 = VECTOR ( 'NONE', #5086, 1000.000000000000000 ) ;
#17076 = CONTEXT_DEPENDENT_SHAPE_REPRESENTATION ( #11728, #13336 ) ;
#17077 = CARTESIAN_POINT ( 'NONE',  ( 9.926985991717000246, -3578.860012824000023, 2250.236835079999764 ) ) ;
#17078 = CIRCLE ( 'NONE', #20452, 5.460999999999938126 ) ;
#17079 = CARTESIAN_POINT ( 'NONE',  ( 25.39999999999999858, -3578.860000000000127, 2247.392000000000280 ) ) ;
#17080 = CARTESIAN_POINT ( 'NONE',  ( 18.22723190021353545, -3660.957995005359862, 2244.667224069949043 ) ) ;
#17081 = CARTESIAN_POINT ( 'NONE',  ( 15.49601198374999989, -3658.956622429000163, 2257.950097350999840 ) ) ;
#17082 = DIRECTION ( 'NONE',  ( 0.000000000000000000, 0.000000000000000000, 1.000000000000000000 ) ) ;
#17083 = CARTESIAN_POINT ( 'NONE',  ( -8.890000000008999592, -3581.552400000000034, 2247.392000000000280 ) ) ;
#17084 = ORIENTED_EDGE ( 'NONE', *, *, #9392, .F. ) ;
#17085 = CIRCLE ( 'NONE', #20105, 4.114799999999974034 ) ;
#17086 = CARTESIAN_POINT ( 'NONE',  ( 7.276271050567447496, -3657.703743155135726, 2245.923136281652205 ) ) ;
#17087 = PRODUCT_DEFINITION ( 'UNKNOWN', '', #7499, #345 ) ;
#17088 = VECTOR ( 'NONE', #22174, 1000.000000000000000 ) ;
#17089 = DIRECTION ( 'NONE',  ( -0.8660254037816071948, 0.5000000000049040771, 0.000000000000000000 ) ) ;
#17090 = VERTEX_POINT ( 'NONE', #13401 ) ;
#17091 = CARTESIAN_POINT ( 'NONE',  ( 60.96000000000000085, -3543.299999999999727, 2279.827800000000025 ) ) ;
#17092 = FACE_OUTER_BOUND ( 'NONE', #19027, .T. ) ;
#17093 = VERTEX_POINT ( 'NONE', #7898 ) ;
#17094 = EDGE_LOOP ( 'NONE', ( #11373, #13437, #4234, #677 ) ) ;
#17095 = EDGE_CURVE ( 'NONE', #1923, #9353, #4487, .T. ) ;
#17096 = ORIENTED_EDGE ( 'NONE', *, *, #18084, .T. ) ;
#17097 = COORDINATED_UNIVERSAL_TIME_OFFSET ( 0, 0, .AHEAD. ) ;
#17098 = DIRECTION ( 'NONE',  ( 1.000000000000000000, 0.000000000000000000, -2.336881798971000105E-14 ) ) ;
#17099 = VECTOR ( 'NONE', #9953, 999.9999999999998863 ) ;
#17100 = ADVANCED_FACE ( 'NONE', ( #11624 ), #6146, .F. ) ;
#17101 = ORIENTED_EDGE ( 'NONE', *, *, #5643, .T. ) ;
#17102 = EDGE_CURVE ( 'NONE', #20980, #7476, #7972, .T. ) ;
#17103 = CARTESIAN_POINT ( 'NONE',  ( 134.2390000000000043, -3579.494999999999891, 2239.391000000000076 ) ) ;
#17104 = CARTESIAN_POINT ( 'NONE',  ( 127.0000000000000000, -3619.500000000000000, 2239.771999999999935 ) ) ;
#17105 = APPLICATION_PROTOCOL_DEFINITION ( 'international standard', 'automotive_design', 2000, #1225 ) ;
#17106 = CARTESIAN_POINT ( 'NONE',  ( 142.0458560721536116, -3581.104231592735687, 2249.140446724335561 ) ) ;
#17107 = ORIENTED_EDGE ( 'NONE', *, *, #17536, .T. ) ;
#17108 = FACE_OUTER_BOUND ( 'NONE', #110, .T. ) ;
#17109 = PERSON_AND_ORGANIZATION ( #5446, #1895 ) ;
#17110 = AXIS2_PLACEMENT_3D ( 'NONE', #10546, #21221, #12310 ) ;
#17111 = DIRECTION ( 'NONE',  ( -2.334777064352623371E-14, -1.000000000000000000, 0.000000000000000000 ) ) ;
#17112 = CARTESIAN_POINT ( 'NONE',  ( -0.7620000000000000107, -3660.140000000000327, 2247.392000000000280 ) ) ;
#17113 = AXIS2_PLACEMENT_3D ( 'NONE', #5145, #98, #23052 ) ;
#17114 = CARTESIAN_POINT ( 'NONE',  ( 134.1174645519585908, -3658.281435122416497, 2245.237728517810865 ) ) ;
#17115 = AXIS2_PLACEMENT_3D ( 'NONE', #10922, #22983, #14565 ) ;
#17116 = EDGE_CURVE ( 'NONE', #12626, #8199, #21805, .T. ) ;
#17117 = ORIENTED_EDGE ( 'NONE', *, *, #11212, .T. ) ;
#17118 = CARTESIAN_POINT ( 'NONE',  ( 142.0222535324996898, -3661.148760393995417, 2250.052190083144069 ) ) ;
#17119 = ORIENTED_EDGE ( 'NONE', *, *, #5212, .F. ) ;
#17120 = EDGE_LOOP ( 'NONE', ( #21853, #22334 ) ) ;
#17121 = AXIS2_PLACEMENT_3D ( 'NONE', #20487, #2333, #7840 ) ;
#17122 = ORIENTED_EDGE ( 'NONE', *, *, #6267, .T. ) ;
#17123 = CARTESIAN_POINT ( 'NONE',  ( -12.69999999999999929, -3580.426170452999941, 2250.104686796999886 ) ) ;
#17124 = CARTESIAN_POINT ( 'NONE',  ( -0.7620000000000000107, -3694.938000000000102, 2239.771999999999935 ) ) ;
#17125 = EDGE_LOOP ( 'NONE', ( #18276, #15443, #2732, #13236 ) ) ;
#17126 = AXIS2_PLACEMENT_3D ( 'NONE', #4607, #22522, #13510 ) ;
#17127 = EDGE_CURVE ( 'NONE', #3088, #18712, #10582, .T. ) ;
#17128 = CARTESIAN_POINT ( 'NONE',  ( 12.69999999999999929, -3579.494999999999891, 2246.630000000000109 ) ) ;
#17129 =( NAMED_UNIT ( * ) SI_UNIT ( $, .STERADIAN. ) SOLID_ANGLE_UNIT ( ) );
#17130 = CARTESIAN_POINT ( 'NONE',  ( 0.000000000000000000, -3694.938000000000102, 2275.763800000000174 ) ) ;
#17131 = DIRECTION ( 'NONE',  ( 0.000000000000000000, 0.000000000000000000, -1.000000000000000000 ) ) ;
#17132 = APPROVAL_ROLE ( '' ) ;
#17133 = EDGE_CURVE ( 'NONE', #17093, #10895, #9584, .T. ) ;
#17134 = ADVANCED_FACE ( 'NONE', ( #17605 ), #18903, .T. ) ;
#17135 = DIRECTION ( 'NONE',  ( -0.5000000000031962211, 0.8660254037825932949, 0.000000000000000000 ) ) ;
#17136 = DIRECTION ( 'NONE',  ( 0.000000000000000000, 0.000000000000000000, 1.000000000000000000 ) ) ;
#17137 = VERTEX_POINT ( 'NONE', #2850 ) ;
#17138 = CARTESIAN_POINT ( 'NONE',  ( 139.6999999999999886, -3579.494999999999891, 2239.009999999999764 ) ) ;
#17139 = DIRECTION ( 'NONE',  ( 0.000000000000000000, -1.000000000000000000, 0.000000000000000000 ) ) ;
#17140 = AXIS2_PLACEMENT_3D ( 'NONE', #1313, #14217, #12104 ) ;
#17141 = DIRECTION ( 'NONE',  ( -1.000000000000000000, 0.000000000000000000, 0.000000000000000000 ) ) ;
#17142 = EDGE_CURVE ( 'NONE', #7229, #13759, #2964, .T. ) ;
#17143 = ORIENTED_EDGE ( 'NONE', *, *, #8064, .T. ) ;
#17144 = CARTESIAN_POINT ( 'NONE',  ( 137.1599999999999966, -3580.776127254000130, 2255.774000000000342 ) ) ;
#17145 = ORIENTED_EDGE ( 'NONE', *, *, #12695, .F. ) ;
#17146 = ORIENTED_EDGE ( 'NONE', *, *, #3981, .F. ) ;
#17147 = EDGE_CURVE ( 'NONE', #17031, #18172, #9815, .T. ) ;
#17148 = CARTESIAN_POINT ( 'NONE',  ( 4.931849146582301557, -3695.327183876642721, 2260.228917875151637 ) ) ;
#17149 = DIRECTION ( 'NONE',  ( 1.000000000000000000, 0.000000000000000000, 0.000000000000000000 ) ) ;
#17150 = ORIENTED_EDGE ( 'NONE', *, *, #3640, .F. ) ;
#17151 = VERTEX_POINT ( 'NONE', #17254 ) ;
#17152 = DIRECTION ( 'NONE',  ( 0.000000000000000000, 0.000000000000000000, 1.000000000000000000 ) ) ;
#17153 = CARTESIAN_POINT ( 'NONE',  ( 12.69999999999999929, -3639.502500000000055, 2263.571799999999712 ) ) ;
#17154 = FACE_OUTER_BOUND ( 'NONE', #4819, .T. ) ;
#17155 = ORIENTED_EDGE ( 'NONE', *, *, #17665, .F. ) ;
#17156 = CARTESIAN_POINT ( 'NONE',  ( 12.69999999999999929, -3599.497499999999945, 2288.971800000000258 ) ) ;
#17157 = CARTESIAN_POINT ( 'NONE',  ( 12.70000000002640661, -3576.802599999840822, 2239.167815367326057 ) ) ;
#17158 = CARTESIAN_POINT ( 'NONE',  ( 18.29277998665192939, -3578.277056357326273, 2244.591048105684877 ) ) ;
#17159 = CIRCLE ( 'NONE', #10426, 0.7619999999999294005 ) ;
#17160 = DIRECTION ( 'NONE',  ( 0.000000000000000000, -1.000000000000000000, 0.000000000000000000 ) ) ;
#17161 = EDGE_LOOP ( 'NONE', ( #10376, #2571, #14958, #18757 ) ) ;
#17162 = APPROVAL_ROLE ( '' ) ;
#17163 = EDGE_CURVE ( 'NONE', #16275, #16505, #9176, .T. ) ;
#17164 = ORIENTED_EDGE ( 'NONE', *, *, #14305, .F. ) ;
#17165 = CARTESIAN_POINT ( 'NONE',  ( 151.1299999999999955, -3543.299999999999727, 2240.279999999999745 ) ) ;
#17166 = CARTESIAN_POINT ( 'NONE',  ( 10.75008131230051411, -3581.566695960163543, 2248.268778118700538 ) ) ;
#17167 = CARTESIAN_POINT ( 'NONE',  ( 101.5999999999999943, -3619.500000000000000, 2239.771999999999935 ) ) ;
#17168 = EDGE_LOOP ( 'NONE', ( #21713, #1678, #12067, #3169 ) ) ;
#17169 = DIRECTION ( 'NONE',  ( -5.682243826821398966E-14, -1.000000000000000000, 0.000000000000000000 ) ) ;
#17170 = DIRECTION ( 'NONE',  ( 0.000000000000000000, -1.000000000000000000, 0.000000000000000000 ) ) ;
#17171 = CARTESIAN_POINT ( 'NONE',  ( 145.2092688553343578, -3661.024727042168252, 2244.688205607526015 ) ) ;
#17172 = VERTEX_POINT ( 'NONE', #278 ) ;
#17173 = VECTOR ( 'NONE', #15905, 1000.000000000000000 ) ;
#17174 = CARTESIAN_POINT ( 'NONE',  ( 12.69999999999133955, -3602.189900000167654, 2296.433984632682041 ) ) ;
#17175 = ADVANCED_FACE ( 'NONE', ( #21604 ), #14569, .F. ) ;
#17176 = CARTESIAN_POINT ( 'NONE',  ( 13.55331166973191159, -3662.218869883657135, 2249.333995280556792 ) ) ;
#17177 = DIRECTION ( 'NONE',  ( -2.336881798971000105E-14, 0.000000000000000000, -1.000000000000000000 ) ) ;
#17178 = ORIENTED_EDGE ( 'NONE', *, *, #22712, .F. ) ;
#17179 = FACE_OUTER_BOUND ( 'NONE', #12628, .T. ) ;
#17180 = DIRECTION ( 'NONE',  ( -1.000000000000000000, 0.000000000000000000, 0.000000000000000000 ) ) ;
#17181 = DIRECTION ( 'NONE',  ( 0.000000000000000000, 0.000000000000000000, -1.000000000000000000 ) ) ;
#17182 = FACE_OUTER_BOUND ( 'NONE', #20411, .T. ) ;
#17183 = DIRECTION ( 'NONE',  ( -1.000000000000000000, 0.000000000000000000, 0.000000000000000000 ) ) ;
#17184 = ORIENTED_EDGE ( 'NONE', *, *, #13682, .T. ) ;
#17185 = VERTEX_POINT ( 'NONE', #16204 ) ;
#17186 = CIRCLE ( 'NONE', #8215, 2.844800000000091700 ) ;
#17187 = CARTESIAN_POINT ( 'NONE',  ( 9.987313202947220248, -3601.063670452640054, 2296.591799999999694 ) ) ;
#17188 = SECURITY_CLASSIFICATION ( '', '', #17357 ) ;
#17189 = EDGE_LOOP ( 'NONE', ( #3727, #7741, #5667, #20382, #16998 ) ) ;
#17190 = B_SPLINE_CURVE_WITH_KNOTS ( 'NONE', 3,
 ( #4095, #16402, #7844, #2459, #13115, #20047 ),
 .UNSPECIFIED., .F., .F.,
 ( 4, 1, 1, 4 ),
 ( 0.000000000000000000, 0.3333333333333000081, 0.6666666666667000474, 1.000000000000000000 ),
 .UNSPECIFIED. ) ;
#17191 = LINE ( 'NONE', #19314, #11150 ) ;
#17192 = APPROVAL_STATUS ( 'not_yet_approved' ) ;
#17193 = APPROVAL ( #52, 'UNKNOWN' ) ;
#17194 = FACE_OUTER_BOUND ( 'NONE', #10532, .T. ) ;
#17195 = PLANE ( 'NONE',  #2251 ) ;
#17196 = CARTESIAN_POINT ( 'NONE',  ( 10.49449033964999956, -3661.309265058999699, 2257.813191440000082 ) ) ;
#17197 = DIRECTION ( 'NONE',  ( -5.197384013923999056E-14, 1.000000000000000000, 0.000000000000000000 ) ) ;
#17198 = DIRECTION ( 'NONE',  ( 0.000000000000000000, 0.000000000000000000, -1.000000000000000000 ) ) ;
#17199 = CARTESIAN_POINT ( 'NONE',  ( 137.3069051741637736, -3577.956663428028151, 2250.089631299345911 ) ) ;
#17200 = ORIENTED_EDGE ( 'NONE', *, *, #22684, .T. ) ;
#17201 = AXIS2_PLACEMENT_3D ( 'NONE', #3284, #16055, #9142 ) ;
#17202 = FACE_OUTER_BOUND ( 'NONE', #20407, .T. ) ;
#17203 = ORIENTED_EDGE ( 'NONE', *, *, #133, .F. ) ;
#17204 = APPROVAL_PERSON_ORGANIZATION ( #490, #5337, #9403 ) ;
#17205 = DIRECTION ( 'NONE',  ( -2.343004830739999973E-14, -1.784212334590129905E-30, -1.000000000000000000 ) ) ;
#17206 = CARTESIAN_POINT ( 'NONE',  ( 10.57571262906792420, -3657.612833920940830, 2248.698263331576527 ) ) ;
#17207 = ORIENTED_EDGE ( 'NONE', *, *, #16436, .T. ) ;
#17208 = ORIENTED_EDGE ( 'NONE', *, *, #18278, .T. ) ;
#17209 = CARTESIAN_POINT ( 'NONE',  ( 134.1971129226658377, -3581.033299165523658, 2245.555178679493565 ) ) ;
#17210 = PRODUCT_DEFINITION_CONTEXT ( 'detailed design', #4108, 'design' ) ;
#17211 = ORIENTED_EDGE ( 'NONE', *, *, #15296, .F. ) ;
#17212 = PRODUCT_DEFINITION_SHAPE ( 'NONE', 'NONE',  #10933 ) ;
#17213 = DIRECTION ( 'NONE',  ( 0.000000000000000000, 0.000000000000000000, 1.000000000000000000 ) ) ;
#17214 = CARTESIAN_POINT ( 'NONE',  ( 95.25000000000000000, -3568.700000000000273, 2247.392000000000280 ) ) ;
#17215 = CARTESIAN_POINT ( 'NONE',  ( 142.3245498262872388, -3580.592634219400679, 2249.648323945948505 ) ) ;
#17216 = EDGE_LOOP ( 'NONE', ( #4974, #17155, #3103, #533 ) ) ;
#17217 = DIRECTION ( 'NONE',  ( 0.6887494619147179753, 0.000000000000000000, -0.7249994335943901191 ) ) ;
#17218 = APPROVAL_ROLE ( '' ) ;
#17219 = APPLIED_PERSON_AND_ORGANIZATION_ASSIGNMENT ( #13752, #1310, ( #381 ) ) ;
#17220 = DIRECTION ( 'NONE',  ( 0.000000000000000000, -1.000000000000000000, 0.000000000000000000 ) ) ;
#17221 = APPLIED_SECURITY_CLASSIFICATION_ASSIGNMENT ( #6021, ( #23166 ) ) ;
#17222 = CARTESIAN_POINT ( 'NONE',  ( 14.61878770176556053, -3581.595291073398130, 2248.174049405876758 ) ) ;
#17223 = APPROVAL_PERSON_ORGANIZATION ( #4405, #4352, #17043 ) ;
#17224 = CARTESIAN_POINT ( 'NONE',  ( 134.0114081857246617, -3658.956231532004949, 2244.804996324768126 ) ) ;
#17225 = ADVANCED_FACE ( 'NONE', ( #12339 ), #1794, .T. ) ;
#17226 = EDGE_CURVE ( 'NONE', #22243, #12173, #3982, .T. ) ;
#17227 = VERTEX_POINT ( 'NONE', #2592 ) ;
#17228 = CARTESIAN_POINT ( 'NONE',  ( 12.69999999999999929, -3599.497499999999945, 2264.841800000000148 ) ) ;
#17229 = ADVANCED_FACE ( 'NONE', ( #18529 ), #13195, .T. ) ;
#17230 = PLANE ( 'NONE',  #17021 ) ;
#17231 = ORIENTED_EDGE ( 'NONE', *, *, #15685, .T. ) ;
#17232 = DIRECTION ( 'NONE',  ( -1.000000000000000000, 0.000000000000000000, 0.000000000000000000 ) ) ;
#17233 = CARTESIAN_POINT ( 'NONE',  ( 19.05000000000000071, -3663.315000000000509, 2247.392000000000280 ) ) ;
#17234 = VERTEX_POINT ( 'NONE', #7990 ) ;
#17235 = ORIENTED_EDGE ( 'NONE', *, *, #18673, .T. ) ;
#17236 = EDGE_CURVE ( 'NONE', #16534, #21188, #20666, .T. ) ;
#17237 = ORIENTED_EDGE ( 'NONE', *, *, #693, .T. ) ;
#17238 = LOCAL_TIME ( 17, 37, 43.00000000000000000, #3133 ) ;
#17239 = CARTESIAN_POINT ( 'NONE',  ( 20.62424768829000143, -3544.570000000000164, 2260.600000000000364 ) ) ;
#17240 = CARTESIAN_POINT ( 'NONE',  ( 12.69999999999999929, -3656.329999999999472, 2270.760000000000218 ) ) ;
#17241 = APPLIED_APPROVAL_ASSIGNMENT ( #14387, ( #6402 ) ) ;
#17242 = VERTEX_POINT ( 'NONE', #13143 ) ;
#17243 = CARTESIAN_POINT ( 'NONE',  ( 0.000000000000000000, -3694.938000000000102, 2295.829799999999977 ) ) ;
#17244 = FACE_OUTER_BOUND ( 'NONE', #19280, .T. ) ;
#17245 = CARTESIAN_POINT ( 'NONE',  ( 14.93205397128999934, -3601.271132144000148, 2279.591813953999463 ) ) ;
#17246 = EDGE_CURVE ( 'NONE', #17616, #3685, #6011, .T. ) ;
#17247 = CARTESIAN_POINT ( 'NONE',  ( 12.69999999999999929, -3594.036500000000160, 2290.622800000000097 ) ) ;
#17248 = APPROVAL_DATE_TIME ( #17483, #18949 ) ;
#17249 = EDGE_CURVE ( 'NONE', #3316, #2186, #2490, .T. ) ;
#17250 = VECTOR ( 'NONE', #15757, 1000.000000000000000 ) ;
#17251 = DIRECTION ( 'NONE',  ( 0.000000000000000000, -1.000000000000000000, 0.000000000000000000 ) ) ;
#17252 = DIRECTION ( 'NONE',  ( 1.000000000000000000, 0.000000000000000000, 0.000000000000000000 ) ) ;
#17253 = CARTESIAN_POINT ( 'NONE',  ( 142.2400000000000091, -3695.699999999999818, 2255.774000000000342 ) ) ;
#17254 = CARTESIAN_POINT ( 'NONE',  ( 151.4000000000000057, -3578.860000000000127, 2244.518167364599321 ) ) ;
#17255 = ORIENTED_EDGE ( 'NONE', *, *, #19982, .F. ) ;
#17256 = EDGE_LOOP ( 'NONE', ( #19054, #6228, #5835, #21304 ) ) ;
#17257 = CARTESIAN_POINT ( 'NONE',  ( 137.0971312009782253, -3543.951823054724173, 2255.616383244340341 ) ) ;
#17258 = ADVANCED_FACE ( 'NONE', ( #16882 ), #7638, .T. ) ;
#17259 = ORIENTED_EDGE ( 'NONE', *, *, #5959, .T. ) ;
#17260 = CIRCLE ( 'NONE', #17635, 2.844800000000001550 ) ;
#17261 = CARTESIAN_POINT ( 'NONE',  ( 4.918032642227820439, -3695.360820973939099, 2260.194368632764053 ) ) ;
#17262 = AXIS2_PLACEMENT_3D ( 'NONE', #13154, #22506, #22274 ) ;
#17263 = DIRECTION ( 'NONE',  ( 0.000000000000000000, 0.000000000000000000, 1.000000000000000000 ) ) ;
#17264 = EDGE_LOOP ( 'NONE', ( #6821, #13062, #19264, #10160 ) ) ;
#17265 = ORIENTED_EDGE ( 'NONE', *, *, #20109, .T. ) ;
#17266 = CARTESIAN_POINT ( 'NONE',  ( 139.7000000000068383, -3576.620370510379416, 2239.010000000095715 ) ) ;
#17267 = DIRECTION ( 'NONE',  ( 0.000000000000000000, 0.000000000000000000, 1.000000000000000000 ) ) ;
#17268 = LINE ( 'NONE', #17373, #250 ) ;
#17269 = ORIENTED_EDGE ( 'NONE', *, *, #5637, .F. ) ;
#17270 = DIRECTION ( 'NONE',  ( -1.000000000000000000, 0.000000000000000000, 0.000000000000000000 ) ) ;
#17271 = LINE ( 'NONE', #4977, #5989 ) ;
#17272 = DIRECTION ( 'NONE',  ( 0.000000000000000000, 0.000000000000000000, -1.000000000000000000 ) ) ;
#17273 = CARTESIAN_POINT ( 'NONE',  ( 12.70000000003999929, -3662.197400000000016, 2242.820000000000164 ) ) ;
#17274 = DIRECTION ( 'NONE',  ( 3.547420834900000257E-14, -1.000000000000000000, 0.000000000000000000 ) ) ;
#17275 = ORIENTED_EDGE ( 'NONE', *, *, #21718, .T. ) ;
#17276 = APPROVAL_DATE_TIME ( #22666, #20655 ) ;
#17277 = ORIENTED_EDGE ( 'NONE', *, *, #22247, .F. ) ;
#17278 = DIRECTION ( 'NONE',  ( 0.000000000000000000, 0.000000000000000000, -1.000000000000000000 ) ) ;
#17279 = AXIS2_PLACEMENT_3D ( 'NONE', #17798, #7145, #14293 ) ;
#17280 = CARTESIAN_POINT ( 'NONE',  ( 101.5999999999999943, -3568.700000000000273, 2239.771999999999935 ) ) ;
#17281 = CARTESIAN_POINT ( 'NONE',  ( -6.349999999999999645, -3578.860000000000127, 2247.392000000000280 ) ) ;
#17282 = ORIENTED_EDGE ( 'NONE', *, *, #22253, .F. ) ;
#17283 = CARTESIAN_POINT ( 'NONE',  ( 12.69999999999999929, -3599.497499999999945, 2263.571799999999712 ) ) ;
#17284 = CARTESIAN_POINT ( 'NONE',  ( 79.80679999999999552, -3670.300000000000182, 2259.837999999999738 ) ) ;
#17285 = CARTESIAN_POINT ( 'NONE',  ( 144.8670818688862596, -3661.946559944367436, 2245.194077383999684 ) ) ;
#17286 =( BOUNDED_CURVE ( )  B_SPLINE_CURVE ( 3, ( #11467, #15109, #22235, #6208 ),
 .UNSPECIFIED., .F., .F. ) 
 B_SPLINE_CURVE_WITH_KNOTS ( ( 4, 4 ),
 ( 1.570796326964730927, 3.141592653589766471 ),
 .UNSPECIFIED. ) 
 CURVE ( )  GEOMETRIC_REPRESENTATION_ITEM ( )  RATIONAL_B_SPLINE_CURVE ( ( 1.000000000000000000, 0.8047378541644016892, 0.8047378541644016892, 1.000000000000000000 ) ) 
 REPRESENTATION_ITEM ( '' )  );
#17287 = CARTESIAN_POINT ( 'NONE',  ( 35.56000000000000227, -3568.700000000000273, 2247.392000000000280 ) ) ;
#17288 = AXIS2_PLACEMENT_3D ( 'NONE', #17900, #19658, #3599 ) ;
#17289 = CARTESIAN_POINT ( 'NONE',  ( 12.57171830751316399, -3662.347666198358638, 2249.186210068741730 ) ) ;
#17290 = EDGE_CURVE ( 'NONE', #9582, #10638, #13571, .T. ) ;
#17291 = VERTEX_POINT ( 'NONE', #9630 ) ;
#17292 = EDGE_CURVE ( 'NONE', #10396, #22318, #11523, .T. ) ;
#17293 = AXIS2_PLACEMENT_3D ( 'NONE', #22696, #21189, #17416 ) ;
#17294 = DIRECTION ( 'NONE',  ( 0.000000000000000000, 0.000000000000000000, -1.000000000000000000 ) ) ;
#17295 = CIRCLE ( 'NONE', #820, 1.269999999999882334 ) ;
#17296 = DIRECTION ( 'NONE',  ( 2.822694825533999934E-12, 1.000000000000000000, 0.000000000000000000 ) ) ;
#17297 = AXIS2_PLACEMENT_3D ( 'NONE', #11799, #1369, #17183 ) ;
#17298 = CARTESIAN_POINT ( 'NONE',  ( 8.520495716475997128, -3581.600846411636667, 2246.629997383320188 ) ) ;
#17299 = CARTESIAN_POINT ( 'NONE',  ( 9.866773677518999364, -3599.183293980000144, 2279.450408114000311 ) ) ;
#17300 = CARTESIAN_POINT ( 'NONE',  ( 136.9269649396999853, -3660.140004248000423, 2250.236800000000130 ) ) ;
#17301 = ORIENTED_EDGE ( 'NONE', *, *, #7508, .T. ) ;
#17302 = FACE_OUTER_BOUND ( 'NONE', #12569, .T. ) ;
#17303 = ORIENTED_EDGE ( 'NONE', *, *, #910, .F. ) ;
#17304 = CARTESIAN_POINT ( 'NONE',  ( 9.958091716253592907, -3543.555041880599219, 2255.268543560162470 ) ) ;
#17306 = VECTOR ( 'NONE', #16544, 1000.000000000000000 ) ;
#17305 = DATE_AND_TIME ( #20953, #22823 ) ;
#17307 = EDGE_CURVE ( 'NONE', #18165, #14110, #8338, .T. ) ;
#17308 = CARTESIAN_POINT ( 'NONE',  ( -5.588000000000000078, -3544.061999999999898, 2228.849999999999909 ) ) ;
#17309 = ORIENTED_EDGE ( 'NONE', *, *, #11815, .F. ) ;
#17310 = EDGE_CURVE ( 'NONE', #10748, #2928, #8484, .T. ) ;
#17311 = DIRECTION ( 'NONE',  ( 0.000000000000000000, 0.000000000000000000, -1.000000000000000000 ) ) ;
#17312 = CARTESIAN_POINT ( 'NONE',  ( 11.88126810894999963, -3662.234158427000239, 2257.621768944999985 ) ) ;
#17313 = AXIS2_PLACEMENT_3D ( 'NONE', #9224, #201, #7350 ) ;
#17314 = DIRECTION ( 'NONE',  ( 0.000000000000000000, 0.000000000000000000, -1.000000000000000000 ) ) ;
#17315 = CARTESIAN_POINT ( 'NONE',  ( 101.5999999999999943, -3670.300000000000182, 2239.009999999999764 ) ) ;
#17316 = VECTOR ( 'NONE', #3757, 1000.000000000000000 ) ;
#17317 = CARTESIAN_POINT ( 'NONE',  ( 12.70000000002425899, -3662.197400000083690, 2239.391000000000076 ) ) ;
#17318 = VERTEX_POINT ( 'NONE', #4463 ) ;
#17319 = PLANE ( 'NONE',  #2472 ) ;
#17320 = DIRECTION ( 'NONE',  ( -1.000000000000000000, 0.000000000000000000, 0.000000000000000000 ) ) ;
#17321 = ORIENTED_EDGE ( 'NONE', *, *, #4101, .F. ) ;
#17322 = CARTESIAN_POINT ( 'NONE',  ( 57.14999999999999858, -3694.430000000000291, 2251.506800000000112 ) ) ;
#17323 = CARTESIAN_POINT ( 'NONE',  ( 10.40077585279555450, -3657.828902820233452, 2249.052517041838655 ) ) ;
#17324 = VECTOR ( 'NONE', #12425, 1000.000000000000000 ) ;
#17325 = ORIENTED_EDGE ( 'NONE', *, *, #17983, .F. ) ;
#17326 = ORIENTED_EDGE ( 'NONE', *, *, #7802, .T. ) ;
#17327 = CARTESIAN_POINT ( 'NONE',  ( 139.7000000000063835, -3656.812599999822851, 2239.167815367340609 ) ) ;
#17328 = VERTEX_POINT ( 'NONE', #11603 ) ;
#17329 = DIRECTION ( 'NONE',  ( 0.000000000000000000, 0.000000000000000000, -1.000000000000000000 ) ) ;
#17330 = DIRECTION ( 'NONE',  ( 0.000000000000000000, 0.000000000000000000, 1.000000000000000000 ) ) ;
#17331 = DIRECTION ( 'NONE',  ( 1.000000000000000000, 2.331176954593497545E-12, 0.000000000000000000 ) ) ;
#17332 = VERTEX_POINT ( 'NONE', #18755 ) ;
#17333 = CARTESIAN_POINT ( 'NONE',  ( 136.8737850351059535, -3579.869057567643722, 2257.957974138634654 ) ) ;
#17334 = PERSON_AND_ORGANIZATION ( #5446, #1895 ) ;
#17335 = CARTESIAN_POINT ( 'NONE',  ( -12.69999999999998153, -3658.573829547082369, 2250.104686796773422 ) ) ;
#17336 = CARTESIAN_POINT ( 'NONE',  ( 15.12912523891256278, -3580.975774486991668, 2249.293871663121990 ) ) ;
#17337 = AXIS2_PLACEMENT_3D ( 'NONE', #5694, #16456, #411 ) ;
#17338 = CARTESIAN_POINT ( 'NONE',  ( 134.1931015038649662, -3657.976686104013879, 2245.544188612589551 ) ) ;
#17339 = ORIENTED_EDGE ( 'NONE', *, *, #16588, .T. ) ;
#17340 = CARTESIAN_POINT ( 'NONE',  ( 15.24000000000000021, -3694.430000000000291, 2255.774000000000342 ) ) ;
#17341 = FACE_OUTER_BOUND ( 'NONE', #19823, .T. ) ;
#17342 = ORIENTED_EDGE ( 'NONE', *, *, #79, .T. ) ;
#17343 = FACE_OUTER_BOUND ( 'NONE', #17801, .T. ) ;
#17344 = APPROVAL ( #3508, 'UNSPECIFIED' ) ;
#17345 = LINE ( 'NONE', #11968, #23009 ) ;
#17346 = ORIENTED_EDGE ( 'NONE', *, *, #3643, .T. ) ;
#17347 = CARTESIAN_POINT ( 'NONE',  ( 135.0886139726999886, -3576.119152860999748, 2246.630000000000109 ) ) ;
#17348 = DIRECTION ( 'NONE',  ( 2.324635735433000053E-14, 0.000000000000000000, 1.000000000000000000 ) ) ;
#17349 = AXIS2_PLACEMENT_3D ( 'NONE', #15831, #2231, #2119 ) ;
#17350 = ORIENTED_EDGE ( 'NONE', *, *, #23162, .T. ) ;
#17351 = CARTESIAN_POINT ( 'NONE',  ( 15.50959416859028117, -3659.956910932261053, 2250.231754334763082 ) ) ;
#17352 = EDGE_CURVE ( 'NONE', #1856, #6511, #15446, .T. ) ;
#17353 = CARTESIAN_POINT ( 'NONE',  ( 142.2400000000000091, -3544.570000000000164, 2255.774000000000342 ) ) ;
#17354 = AXIS2_PLACEMENT_3D ( 'NONE', #13296, #15291, #4501 ) ;
#17355 = EDGE_CURVE ( 'NONE', #7476, #15463, #11323, .T. ) ;
#17356 = CARTESIAN_POINT ( 'NONE',  ( -8.890000000017000303, -3658.793800000000374, 2249.723686796999573 ) ) ;
#17357 = SECURITY_CLASSIFICATION_LEVEL ( 'unclassified' ) ;
#17358 = EDGE_CURVE ( 'NONE', #20273, #22341, #6469, .T. ) ;
#17359 = CARTESIAN_POINT ( 'NONE',  ( 15.03168679714000078, -3640.848700000000008, 2292.781800000000203 ) ) ;
#17360 = DIRECTION ( 'NONE',  ( 0.000000000000000000, 0.000000000000000000, 1.000000000000000000 ) ) ;
#17361 = FACE_OUTER_BOUND ( 'NONE', #12896, .T. ) ;
#17362 = CARTESIAN_POINT ( 'NONE',  ( 141.8518928781941213, -3657.644192185515294, 2248.757418371342283 ) ) ;
#17363 = ORIENTED_EDGE ( 'NONE', *, *, #6651, .T. ) ;
#17364 = CIRCLE ( 'NONE', #7286, 11.11249999999999716 ) ;
#17365 = DIRECTION ( 'NONE',  ( -4.457711412217000029E-12, 1.000000000000000000, 0.000000000000000000 ) ) ;
#17366 = AXIS2_PLACEMENT_3D ( 'NONE', #14775, #13124, #18054 ) ;
#17367 = AXIS2_PLACEMENT_3D ( 'NONE', #7317, #5326, #19853 ) ;
#17368 = ORIENTED_EDGE ( 'NONE', *, *, #18859, .T. ) ;
#17369 = DIRECTION ( 'NONE',  ( -1.000000000000000000, 0.000000000000000000, 0.000000000000000000 ) ) ;
#17370 = ORIENTED_EDGE ( 'NONE', *, *, #969, .T. ) ;
#17371 = VERTEX_POINT ( 'NONE', #6702 ) ;
#17372 = CARTESIAN_POINT ( 'NONE',  ( 50.79999999999999716, -3670.300000000000182, 2239.009999999999764 ) ) ;
#17373 = CARTESIAN_POINT ( 'NONE',  ( 151.6380000000000052, -3695.699999999999818, 2280.589800000000196 ) ) ;
#17374 = EDGE_LOOP ( 'NONE', ( #20519, #1326 ) ) ;
#17375 = CARTESIAN_POINT ( 'NONE',  ( 63.50000000000000000, -3644.899999999999636, 2239.009999999999764 ) ) ;
#17376 = ADVANCED_FACE ( 'NONE', ( #20627 ), #7225, .T. ) ;
#17377 = DIRECTION ( 'NONE',  ( 1.000000000000000000, 0.000000000000000000, 0.000000000000000000 ) ) ;
#17378 = DIRECTION ( 'NONE',  ( -1.000000000000000000, 0.000000000000000000, 0.000000000000000000 ) ) ;
#17379 = CIRCLE ( 'NONE', #194, 1.523999999999965160 ) ;
#17380 = CARTESIAN_POINT ( 'NONE',  ( 40.94480000000000075, -3594.099999999999909, 2239.771999999999935 ) ) ;
#17381 = AXIS2_PLACEMENT_3D ( 'NONE', #8864, #16007, #7222 ) ;
#17382 = CYLINDRICAL_SURFACE ( 'NONE', #22297, 0.3809999999999303388 ) ;
#17383 = EDGE_CURVE ( 'NONE', #5385, #4126, #10202, .T. ) ;
#17384 = ORIENTED_EDGE ( 'NONE', *, *, #1847, .F. ) ;
#17385 = APPROVAL_ROLE ( '' ) ;
#17387 = EDGE_CURVE ( 'NONE', #17090, #16534, #573, .T. ) ;
#17386 = AXIS2_PLACEMENT_3D ( 'NONE', #15344, #4795, #4553 ) ;
#17388 = ORIENTED_EDGE ( 'NONE', *, *, #7827, .F. ) ;
#17389 = AXIS2_PLACEMENT_3D ( 'NONE', #6137, #22393, #6365 ) ;
#17390 = CARTESIAN_POINT ( 'NONE',  ( -12.69999999999999929, -3580.426170453010855, 2250.104686796980332 ) ) ;
#17391 = ORIENTED_EDGE ( 'NONE', *, *, #21630, .F. ) ;
#17392 = CARTESIAN_POINT ( 'NONE',  ( 10.45150839067501813, -3581.237797149968173, 2248.953753074173619 ) ) ;
#17393 = DIRECTION ( 'NONE',  ( 0.000000000000000000, 0.000000000000000000, 1.000000000000000000 ) ) ;
#17394 = VERTEX_POINT ( 'NONE', #11722 ) ;
#17395 = CARTESIAN_POINT ( 'NONE',  ( 0.7620000000000000107, -3694.938000000000102, 2275.001800000000003 ) ) ;
#17396 = EDGE_CURVE ( 'NONE', #19707, #11877, #1985, .T. ) ;
#17397 = CIRCLE ( 'NONE', #19661, 3.606800000000000228 ) ;
#17398 = CARTESIAN_POINT ( 'NONE',  ( 41.70680000000000121, -3594.099999999999909, 2260.600000000000364 ) ) ;
#17399 = CARTESIAN_POINT ( 'NONE',  ( 144.4566314728151895, -3662.673839737894014, 2246.096241040939276 ) ) ;
#17400 = CARTESIAN_POINT ( 'NONE',  ( 57.14999999999999858, -3544.570000000000164, 2247.392000000000280 ) ) ;
#17401 = AXIS2_PLACEMENT_3D ( 'NONE', #10411, #3376, #7137 ) ;
#17402 = DIRECTION ( 'NONE',  ( -2.324635735433000053E-14, 0.000000000000000000, -1.000000000000000000 ) ) ;
#17403 = VECTOR ( 'NONE', #13557, 1000.000000000000114 ) ;
#17404 = DIRECTION ( 'NONE',  ( 0.000000000000000000, 0.8660254037820785955, -0.5000000000040877302 ) ) ;
#17405 = AXIS2_PLACEMENT_3D ( 'NONE', #20961, #15926, #3145 ) ;
#17406 = VERTEX_POINT ( 'NONE', #22495 ) ;
#17407 = LINE ( 'NONE', #4052, #546 ) ;
#17408 = CIRCLE ( 'NONE', #6963, 3.175000000000149925 ) ;
#17409 = CARTESIAN_POINT ( 'NONE',  ( 117.9067999999989951, -3644.899999999999636, 2239.771999999999935 ) ) ;
#17410 = DIRECTION ( 'NONE',  ( 0.000000000000000000, 1.000000000000000000, 0.000000000000000000 ) ) ;
#17411 = CARTESIAN_POINT ( 'NONE',  ( 12.69999999999999929, -3648.710000000000036, 2257.592639999999847 ) ) ;
#17412 = DIRECTION ( 'NONE',  ( -1.000000000000000000, 0.000000000000000000, 0.000000000000000000 ) ) ;
#17413 = EDGE_LOOP ( 'NONE', ( #2289, #13287 ) ) ;
#17414 = ORIENTED_EDGE ( 'NONE', *, *, #1529, .T. ) ;
#17415 = ADVANCED_FACE ( 'NONE', ( #19000 ), #2940, .T. ) ;
#17416 = DIRECTION ( 'NONE',  ( -2.848935406719999894E-12, 1.000000000000000000, 0.000000000000000000 ) ) ;
#17417 = AXIS2_PLACEMENT_3D ( 'NONE', #17888, #1836, #12033 ) ;
#17418 = ORIENTED_EDGE ( 'NONE', *, *, #8578, .T. ) ;
#17419 = CARTESIAN_POINT ( 'NONE',  ( 141.9621417935377679, -3657.770058126337062, 2257.824813612040543 ) ) ;
#17420 = AXIS2_PLACEMENT_3D ( 'NONE', #11447, #18703, #9798 ) ;
#17421 = DATE_AND_TIME ( #8994, #1144 ) ;
#17422 = EDGE_CURVE ( 'NONE', #17069, #17829, #10948, .T. ) ;
#17423 = FACE_OUTER_BOUND ( 'NONE', #18008, .T. ) ;
#17424 = AXIS2_PLACEMENT_3D ( 'NONE', #17375, #12244, #19040 ) ;
#17425 = EDGE_CURVE ( 'NONE', #21589, #22478, #13944, .T. ) ;
#17426 = ORIENTED_EDGE ( 'NONE', *, *, #17860, .F. ) ;
#17427 = DIRECTION ( 'NONE',  ( 0.000000000000000000, -1.000000000000000000, 0.000000000000000000 ) ) ;
#17428 = CARTESIAN_POINT ( 'NONE',  ( 10.89501796730999850, -3661.709918484999889, 2257.739459224999791 ) ) ;
#17429 =( BOUNDED_CURVE ( )  B_SPLINE_CURVE ( 3, ( #11504, #7773, #2384, #22050 ),
 .UNSPECIFIED., .F., .F. ) 
 B_SPLINE_CURVE_WITH_KNOTS ( ( 4, 4 ),
 ( -9.769962616701377556E-15, 1.570796326960964162 ),
 .UNSPECIFIED. ) 
 CURVE ( )  GEOMETRIC_REPRESENTATION_ITEM ( )  RATIONAL_B_SPLINE_CURVE ( ( 1.000000000000000000, 0.8047378540852202500, 0.8047378540852202500, 1.000000000000000000 ) ) 
 REPRESENTATION_ITEM ( '' )  );
#17430 = AXIS2_PLACEMENT_3D ( 'NONE', #1940, #9092, #12137 ) ;
#17431 = CARTESIAN_POINT ( 'NONE',  ( 15.24000000000000021, -3660.786127253999894, 2255.774000000000342 ) ) ;
#17432 = FACE_OUTER_BOUND ( 'NONE', #9701, .T. ) ;
#17433 = AXIS2_PLACEMENT_3D ( 'NONE', #22864, #13862, #1311 ) ;
#17434 = DIRECTION ( 'NONE',  ( -2.324635735433000053E-14, 2.336881798971000105E-14, -1.000000000000000000 ) ) ;
#17435 = EDGE_CURVE ( 'NONE', #18295, #22481, #6844, .T. ) ;
#17436 = ORIENTED_EDGE ( 'NONE', *, *, #13438, .F. ) ;
#17437 = CARTESIAN_POINT ( 'NONE',  ( 142.4126867972000241, -3577.928829547000078, 2239.009999999999764 ) ) ;
#17438 = DIRECTION ( 'NONE',  ( -1.000000000000000000, 5.461016542361937364E-28, 2.336881798970999789E-14 ) ) ;
#17439 = ORIENTED_EDGE ( 'NONE', *, *, #1277, .F. ) ;
#17440 = VECTOR ( 'NONE', #2978, 1000.000000000000000 ) ;
#17441 = CARTESIAN_POINT ( 'NONE',  ( 0.000000000000000000, -3544.061999999999898, 2295.829799999999977 ) ) ;
#17442 = CARTESIAN_POINT ( 'NONE',  ( 10.85008925745106723, -3657.343667564798579, 2247.916674758225781 ) ) ;
#17443 = ADVANCED_FACE ( 'NONE', ( #21339 ), #8913, .T. ) ;
#17444 = VECTOR ( 'NONE', #14584, 999.9999999999998863 ) ;
#17445 = EDGE_CURVE ( 'NONE', #19565, #7027, #4242, .T. ) ;
#17446 = ORIENTED_EDGE ( 'NONE', *, *, #1635, .T. ) ;
#17447 = CARTESIAN_POINT ( 'NONE',  ( 12.69999999999981988, -3602.672500000000127, 2290.241799999999785 ) ) ;
#17448 = CIRCLE ( 'NONE', #18575, 1.904999999999823501 ) ;
#17449 = EDGE_LOOP ( 'NONE', ( #12254, #6413, #225, #22624 ) ) ;
#17450 = DIRECTION ( 'NONE',  ( 0.000000000000000000, 0.000000000000000000, -1.000000000000000000 ) ) ;
#17451 = CALENDAR_DATE ( 2026, 26, 10 ) ;
#17452 = CIRCLE ( 'NONE', #16344, 2.844800000000091700 ) ;
#17453 = SPHERICAL_SURFACE ( 'NONE', #4571, 0.7620000000000000107 ) ;
#17454 = B_SPLINE_CURVE_WITH_KNOTS ( 'NONE', 3,
 ( #3506, #5750, #20038, #17684, #11461, #13005, #688, #16619, #20593, #16845, #458, #9370, #14879, #22011, #20154, #15104, #2559, #6089, #9703, #4433, #18613, #14761, #4091, #16506, #2223, #4203, #22228, #900, #18266, #14988, #8068, #7604, #22347, #7954, #5976, #21901, #13451, #2667, #22122, #15217, #6199 ),
 .UNSPECIFIED., .F., .F.,
 ( 4, 2, 2, 1, 1, 2, 2, 2, 2, 1, 1, 1, 2, 2, 2, 2, 2, 2, 2, 1, 1, 2, 2, 4 ),
 ( 0.000000000000000000, 0.1250000000073855644, 0.1875000000110783605, 0.2187500000129247446, 0.2343750000138479228, 0.2421875000143108858, 0.2500000000147738488, 0.3750000000221110352, 0.4375000000258316701, 0.4687500000276899614, 0.4843750000284952617, 0.4921875000288853941, 0.4960937500290684699, 0.5000000000292516011, 0.5625000000271654921, 0.5937500000262729838, 0.6250000000253805865, 0.6875000000235473863, 0.7187500000224613661, 0.7343750000221259677, 0.7421875000219583240, 0.7460937500217790230, 0.7500000000215996110, 1.000000000000000000 ),
 .UNSPECIFIED. ) ;
#17455 = ORIENTED_EDGE ( 'NONE', *, *, #7636, .F. ) ;
#17456 = LINE ( 'NONE', #19105, #4386 ) ;
#17457 = DATE_AND_TIME ( #22376, #14601 ) ;
#17458 = EDGE_CURVE ( 'NONE', #12839, #4608, #16217, .T. ) ;
#17459 = LINE ( 'NONE', #22611, #13377 ) ;
#17460 = CARTESIAN_POINT ( 'NONE',  ( 134.0265221272451015, -3658.817503259591831, 2244.873283007213558 ) ) ;
#17461 = AXIS2_PLACEMENT_3D ( 'NONE', #7894, #6262, #4597 ) ;
#17462 = CARTESIAN_POINT ( 'NONE',  ( 1.270000000000000018, -3660.140000000000327, 2247.392000000000280 ) ) ;
#17463 = EDGE_LOOP ( 'NONE', ( #12814, #4349 ) ) ;
#17464 = AXIS2_PLACEMENT_3D ( 'NONE', #19322, #9819, #906 ) ;
#17465 = AXIS2_PLACEMENT_3D ( 'NONE', #12342, #7189, #3313 ) ;
#17466 = CARTESIAN_POINT ( 'NONE',  ( 15.44190828346374467, -3695.444958118781869, 2255.268543560987382 ) ) ;
#17467 = CARTESIAN_POINT ( 'NONE',  ( 127.0000000000000000, -3670.300000000000182, 2259.837999999999738 ) ) ;
#17468 = ORIENTED_EDGE ( 'NONE', *, *, #14749, .F. ) ;
#17469 = AXIS2_PLACEMENT_3D ( 'NONE', #4567, #22484, #16983 ) ;
#17470 = CARTESIAN_POINT ( 'NONE',  ( 25.39999999999999858, -3660.140000000000327, 2247.392000000000280 ) ) ;
#17471 = EDGE_CURVE ( 'NONE', #16618, #1484, #19579, .T. ) ;
#17472 = DIRECTION ( 'NONE',  ( 1.000000000000000000, 0.000000000000000000, 0.000000000000000000 ) ) ;
#17473 = ORIENTED_EDGE ( 'NONE', *, *, #14031, .T. ) ;
#17474 = FACE_OUTER_BOUND ( 'NONE', #19985, .T. ) ;
#17475 = CARTESIAN_POINT ( 'NONE',  ( 133.9968099895132525, -3659.875514725911216, 2244.559017653038609 ) ) ;
#17476 = EDGE_LOOP ( 'NONE', ( #3330, #18571, #9129, #6933 ) ) ;
#17477 = VECTOR ( 'NONE', #3624, 1000.000000000000000 ) ;
#17478 = CARTESIAN_POINT ( 'NONE',  ( 151.4000000000000057, -3695.670967364599164, 2239.009999999999764 ) ) ;
#17479 = DIRECTION ( 'NONE',  ( 0.000000000000000000, -2.336881798971000105E-14, 1.000000000000000000 ) ) ;
#17480 =( NAMED_UNIT ( * ) PLANE_ANGLE_UNIT ( ) SI_UNIT ( $, .RADIAN. ) );
#17481 = CARTESIAN_POINT ( 'NONE',  ( 38.10000000000000142, -3594.099999999999909, 2239.771999999999935 ) ) ;
#17482 = CARTESIAN_POINT ( 'NONE',  ( 139.6999999999999886, -3659.504999999999654, 2246.630000000000109 ) ) ;
#17483 = DATE_AND_TIME ( #19018, #4105 ) ;
#17484 = CIRCLE ( 'NONE', #19744, 0.7619999999999294005 ) ;
#17485 = CIRCLE ( 'NONE', #7397, 0.7619999999999987894 ) ;
#17486 = DIRECTION ( 'NONE',  ( 0.000000000000000000, 0.000000000000000000, -1.000000000000000000 ) ) ;
#17487 = DIRECTION ( 'NONE',  ( 0.8660254037838025498, -0.5000000000011017853, 0.000000000000000000 ) ) ;
#17488 = B_SPLINE_CURVE_WITH_KNOTS ( 'NONE', 3,
 ( #11362, #13355, #2353, #20385, #13125, #20499, #920, #18628, #16977, #5884, #13021, #16862, #2468, #20165, #4107, #8085 ),
 .UNSPECIFIED., .F., .F.,
 ( 4, 2, 2, 2, 2, 2, 2, 4 ),
 ( 0.01338840031623607721, 0.01394627866515972536, 0.01450415701408337178, 0.01506203536300701820, 0.01561991371193066636, 0.01673567040977796266, 0.01729354875870160735, 0.01785142710762525550 ),
 .UNSPECIFIED. ) ;
#17489 = CARTESIAN_POINT ( 'NONE',  ( 18.40091559669128785, -3579.898563401232423, 2244.742832167099550 ) ) ;
#17490 = CIRCLE ( 'NONE', #9581, 6.349999999999855760 ) ;
#17491 = APPLIED_PERSON_AND_ORGANIZATION_ASSIGNMENT ( #22460, #20594, ( #6021 ) ) ;
#17492 = CARTESIAN_POINT ( 'NONE',  ( 141.4948555334656533, -3657.297722024060022, 2247.260386800592642 ) ) ;
#17493 = ORIENTED_EDGE ( 'NONE', *, *, #12076, .F. ) ;
#17494 = CARTESIAN_POINT ( 'NONE',  ( 15.18950216443630374, -3640.939814744946034, 2296.591800000036528 ) ) ;
#17495 = CIRCLE ( 'NONE', #20492, 5.714999999998998881 ) ;
#17496 = VERTEX_POINT ( 'NONE', #126 ) ;
#17497 = VERTEX_POINT ( 'NONE', #10666 ) ;
#17498 = CARTESIAN_POINT ( 'NONE',  ( 139.6999999999999886, -3579.494999999999891, 2239.391000000000076 ) ) ;
#17499 = EDGE_LOOP ( 'NONE', ( #15503, #15053, #23117, #9857 ) ) ;
#17500 = VERTEX_POINT ( 'NONE', #23076 ) ;
#17501 = CARTESIAN_POINT ( 'NONE',  ( 4.891147941723409609, -3543.580319133069679, 2260.126839620043938 ) ) ;
#17502 = CALENDAR_DATE ( 2026, 26, 10 ) ;
#17503 = LINE ( 'NONE', #3090, #10273 ) ;
#17504 = LINE ( 'NONE', #8842, #11823 ) ;
#17505 = EDGE_LOOP ( 'NONE', ( #9858, #13833, #21205, #6690 ) ) ;
#17506 = CYLINDRICAL_SURFACE ( 'NONE', #10339, 0.7619999999999294005 ) ;
#17507 = DIRECTION ( 'NONE',  ( 0.000000000000000000, 0.000000000000000000, 1.000000000000000000 ) ) ;
#17508 = DIRECTION ( 'NONE',  ( 0.000000000000000000, 0.000000000000000000, 1.000000000000000000 ) ) ;
#17509 = DIRECTION ( 'NONE',  ( 0.000000000000000000, 0.000000000000000000, -1.000000000000000000 ) ) ;
#17510 = ORIENTED_EDGE ( 'NONE', *, *, #6018, .T. ) ;
#17511 = PERSON_AND_ORGANIZATION ( #5446, #1895 ) ;
#17512 = ORIENTED_EDGE ( 'NONE', *, *, #12089, .F. ) ;
#17513 = CARTESIAN_POINT ( 'NONE',  ( 88.90000000000000568, -3644.899999999999636, 2261.869999999999891 ) ) ;
#17514 = APPROVAL ( #2748, 'UNSPECIFIED' ) ;
#17515 = CARTESIAN_POINT ( 'NONE',  ( 10.39560465552007429, -3581.163134149680900, 2249.062244971506061 ) ) ;
#17516 = DIRECTION ( 'NONE',  ( 0.000000000000000000, 1.000000000000000000, 0.000000000000000000 ) ) ;
#17517 = ORIENTED_EDGE ( 'NONE', *, *, #11713, .T. ) ;
#17518 = FACE_BOUND ( 'NONE', #2433, .T. ) ;
#17519 = EDGE_CURVE ( 'NONE', #2160, #7862, #249, .T. ) ;
#17520 = EDGE_CURVE ( 'NONE', #1856, #2862, #22923, .T. ) ;
#17521 = DIRECTION ( 'NONE',  ( -1.000000000000000000, 5.461016542361937364E-28, 2.336881798970999789E-14 ) ) ;
#17522 = CARTESIAN_POINT ( 'NONE',  ( 144.4360977138962312, -3576.295496202077629, 2246.158276164633662 ) ) ;
#17523 = DIRECTION ( 'NONE',  ( 0.000000000000000000, 0.000000000000000000, -1.000000000000000000 ) ) ;
#17524 = CARTESIAN_POINT ( 'NONE',  ( 10.34485765540272162, -3661.108525532338717, 2250.070618451575683 ) ) ;
#17525 = EDGE_CURVE ( 'NONE', #8533, #1451, #22960, .T. ) ;
#17526 = CARTESIAN_POINT ( 'NONE',  ( 147.3450752001671447, -3544.173420539331801, 2260.537168198814925 ) ) ;
#17527 = ORIENTED_EDGE ( 'NONE', *, *, #13406, .T. ) ;
#17528 = B_SPLINE_CURVE_WITH_KNOTS ( 'NONE', 3,
 ( #1995, #17570, #122, #19343 ),
 .UNSPECIFIED., .F., .F.,
 ( 4, 4 ),
 ( 0.000000000000000000, 1.000000000000000000 ),
 .UNSPECIFIED. ) ;
#17529 = AXIS2_PLACEMENT_3D ( 'NONE', #3728, #18033, #19561 ) ;
#17530 = FACE_OUTER_BOUND ( 'NONE', #551, .T. ) ;
#17531 = CARTESIAN_POINT ( 'NONE',  ( 137.3683132029000262, -3580.841199999999844, 2242.820000000000164 ) ) ;
#17532 = CARTESIAN_POINT ( 'NONE',  ( 14.76142536199160560, -3657.543251715168935, 2248.559521133435737 ) ) ;
#17533 = EDGE_CURVE ( 'NONE', #14578, #5209, #17575, .T. ) ;
#17534 = CARTESIAN_POINT ( 'NONE',  ( 20.32000000000000028, -3670.300000000000182, 2292.057900000000245 ) ) ;
#17535 = ORIENTED_EDGE ( 'NONE', *, *, #16811, .T. ) ;
#17536 = EDGE_CURVE ( 'NONE', #8499, #15888, #19576, .T. ) ;
#17537 = ORIENTED_EDGE ( 'NONE', *, *, #10557, .F. ) ;
#17538 = DIRECTION ( 'NONE',  ( 0.000000000000000000, 0.000000000000000000, -1.000000000000000000 ) ) ;
#17539 = ADVANCED_FACE ( 'NONE', ( #21574 ), #1233, .T. ) ;
#17540 = EDGE_LOOP ( 'NONE', ( #16182, #157, #5316, #1654 ) ) ;
#17541 = CARTESIAN_POINT ( 'NONE',  ( 9.832492551972105588, -3543.382189094968908, 2254.953947932267056 ) ) ;
#17542 = CARTESIAN_POINT ( 'NONE',  ( 57.14999999999999858, -3544.570000000000164, 2251.506800000000112 ) ) ;
#17543 = CARTESIAN_POINT ( 'NONE',  ( 11.12270644712000056, -3657.131901141000071, 2257.704293189000055 ) ) ;
#17544 = LINE ( 'NONE', #5022, #15196 ) ;
#17545 = VECTOR ( 'NONE', #1952, 1000.000000000000000 ) ;
#17546 = DIRECTION ( 'NONE',  ( 0.000000000000000000, 0.000000000000000000, -1.000000000000000000 ) ) ;
#17547 = CARTESIAN_POINT ( 'NONE',  ( 139.6999999999999886, -3579.494999999999891, 2239.009999999999764 ) ) ;
#17548 = LINE ( 'NONE', #443, #15492 ) ;
#17549 = ORIENTED_EDGE ( 'NONE', *, *, #7721, .F. ) ;
#17550 = DIRECTION ( 'NONE',  ( 0.000000000000000000, 0.000000000000000000, 1.000000000000000000 ) ) ;
#17551 = EDGE_CURVE ( 'NONE', #11149, #8967, #1764, .T. ) ;
#17552 = CARTESIAN_POINT ( 'NONE',  ( 12.69999999999999929, -3639.502500000000055, 2290.241799999999785 ) ) ;
#17553 = ORIENTED_EDGE ( 'NONE', *, *, #2787, .F. ) ;
#17554 = CARTESIAN_POINT ( 'NONE',  ( 6.985000000000000320, -3659.504999999999654, 2246.630000000000109 ) ) ;
#17555 = CARTESIAN_POINT ( 'NONE',  ( 130.6067999999989979, -3670.300000000000182, 2260.600000000000364 ) ) ;
#17556 = EDGE_CURVE ( 'NONE', #1252, #13105, #2720, .T. ) ;
#17557 = EDGE_CURVE ( 'NONE', #18372, #13470, #12544, .T. ) ;
#17558 = ORIENTED_EDGE ( 'NONE', *, *, #17658, .F. ) ;
#17559 = CARTESIAN_POINT ( 'NONE',  ( 134.3871257470999865, -3581.600847139000052, 2246.630000000000109 ) ) ;
#17560 = CIRCLE ( 'NONE', #10846, 6.477000000001009283 ) ;
#17561 = ORIENTED_EDGE ( 'NONE', *, *, #8524, .F. ) ;
#17562 = EDGE_LOOP ( 'NONE', ( #13938, #5788, #13227, #14504 ) ) ;
#17563 = CARTESIAN_POINT ( 'NONE',  ( 3.048000000000000043, -3695.699999999999818, 2229.612000000000080 ) ) ;
#17564 = PERSON_AND_ORGANIZATION ( #5446, #1895 ) ;
#17565 = DIRECTION ( 'NONE',  ( 1.163002179513000119E-14, 1.000000000000000000, 9.924285265180999807E-13 ) ) ;
#17566 = ORIENTED_EDGE ( 'NONE', *, *, #18717, .F. ) ;
#17567 = CARTESIAN_POINT ( 'NONE',  ( 131.8393559128971049, -3695.512751957134697, 2259.997167822851679 ) ) ;
#17568 =( BOUNDED_CURVE ( )  B_SPLINE_CURVE ( 3, ( #17033, #17266, #983, #10010 ),
 .UNSPECIFIED., .F., .T. ) 
 B_SPLINE_CURVE_WITH_KNOTS ( ( 4, 4 ),
 ( 1.570796327224941002, 3.141592653589829531 ),
 .UNSPECIFIED. ) 
 CURVE ( )  GEOMETRIC_REPRESENTATION_ITEM ( )  RATIONAL_B_SPLINE_CURVE ( ( 1.000000000000000000, 0.8047378542257188627, 0.8047378542257188627, 1.000000000000000000 ) ) 
 REPRESENTATION_ITEM ( '' )  );
#17569 = DATE_TIME_ROLE ( 'creation_date' ) ;
#17570 = CARTESIAN_POINT ( 'NONE',  ( 6.985000002048997736, -3579.284482508065139, 2244.570813839142829 ) ) ;
#17571 = CARTESIAN_POINT ( 'NONE',  ( 15.47643293920226526, -3580.121238382759202, 2249.943944374062085 ) ) ;
#17572 = ADVANCED_FACE ( 'NONE', ( #8682 ), #21680, .T. ) ;
#17573 = AXIS2_PLACEMENT_3D ( 'NONE', #12192, #10548, #21223 ) ;
#17574 = CARTESIAN_POINT ( 'NONE',  ( 146.1770000000009873, -3579.494999999999891, 2239.009999999999764 ) ) ;
#17575 = LINE ( 'NONE', #3741, #17324 ) ;
#17576 = APPLIED_SECURITY_CLASSIFICATION_ASSIGNMENT ( #6739, ( #3730 ) ) ;
#17577 = ORIENTED_EDGE ( 'NONE', *, *, #13409, .F. ) ;
#17578 = CARTESIAN_POINT ( 'NONE',  ( 116.8400000000000034, -3568.700000000000273, 2247.392000000000280 ) ) ;
#17579 = CARTESIAN_POINT ( 'NONE',  ( 12.79208108087000006, -3576.650200000000041, 2257.592639999999847 ) ) ;
#17580 = ORIENTED_EDGE ( 'NONE', *, *, #19120, .F. ) ;
#17581 = ORIENTED_EDGE ( 'NONE', *, *, #14655, .F. ) ;
#17582 = DIRECTION ( 'NONE',  ( 0.000000000000000000, 0.000000000000000000, -1.000000000000000000 ) ) ;
#17583 = EDGE_CURVE ( 'NONE', #7868, #8915, #15829, .T. ) ;
#17584 = CARTESIAN_POINT ( 'NONE',  ( 12.70000000000865903, -3662.197400000167818, 2239.167815367317871 ) ) ;
#17585 = VERTEX_POINT ( 'NONE', #15944 ) ;
#17586 = ORIENTED_EDGE ( 'NONE', *, *, #19156, .F. ) ;
#17587 = DIRECTION ( 'NONE',  ( 0.000000000000000000, 0.000000000000000000, 1.000000000000000000 ) ) ;
#17588 = CARTESIAN_POINT ( 'NONE',  ( 134.0107419914343154, -3660.047848187909040, 2244.548477525994713 ) ) ;
#17589 = CIRCLE ( 'NONE', #11240, 3.606799999999001027 ) ;
#17590 = VERTEX_POINT ( 'NONE', #7053 ) ;
#17591 = CARTESIAN_POINT ( 'NONE',  ( -0.7620000000000000107, -3578.860000000000127, 2247.392000000000280 ) ) ;
#17592 = CARTESIAN_POINT ( 'NONE',  ( 124.1552000000010025, -3670.300000000000182, 2259.837999999999738 ) ) ;
#17593 = CARTESIAN_POINT ( 'NONE',  ( 60.65520000000000067, -3594.099999999999909, 2261.869999999999891 ) ) ;
#17594 = APPLIED_SECURITY_CLASSIFICATION_ASSIGNMENT ( #13118, ( #8248 ) ) ;
#17595 = ADVANCED_FACE ( 'NONE', ( #7609 ), #18089, .T. ) ;
#17596 = LOCAL_TIME ( 17, 37, 43.00000000000000000, #11207 ) ;
#17597 = DIRECTION ( 'NONE',  ( 0.000000000000000000, 0.000000000000000000, 1.000000000000000000 ) ) ;
#17598 = APPROVAL_ROLE ( '' ) ;
#17599 = DIRECTION ( 'NONE',  ( 0.000000000000000000, 0.000000000000000000, 1.000000000000000000 ) ) ;
#17600 = CIRCLE ( 'NONE', #11249, 0.7619999999999294005 ) ;
#17601 = CARTESIAN_POINT ( 'NONE',  ( 9.698254031360443506, -3695.699999999987995, 2254.617539518482772 ) ) ;
#17602 = CARTESIAN_POINT ( 'NONE',  ( 18.34588546172644996, -3580.386202656615751, 2244.987819353370014 ) ) ;
#17603 = EDGE_CURVE ( 'NONE', #7997, #2236, #2189, .T. ) ;
#17604 = EDGE_CURVE ( 'NONE', #10320, #6015, #2460, .T. ) ;
#17605 = FACE_OUTER_BOUND ( 'NONE', #5854, .T. ) ;
#17606 = EDGE_CURVE ( 'NONE', #13352, #6776, #20333, .T. ) ;
#17607 = ORIENTED_EDGE ( 'NONE', *, *, #9071, .T. ) ;
#17608 = DIRECTION ( 'NONE',  ( 1.000000000000000000, 0.000000000000000000, 0.000000000000000000 ) ) ;
#17609 = ORIENTED_EDGE ( 'NONE', *, *, #7813, .F. ) ;
#17610 = ORIENTED_EDGE ( 'NONE', *, *, #14305, .T. ) ;
#17611 = CARTESIAN_POINT ( 'NONE',  ( 116.8400000000000034, -3694.430000000000291, 2243.277199999999993 ) ) ;
#17612 = APPLIED_APPROVAL_ASSIGNMENT ( #18237, ( #18354 ) ) ;
#17613 = ORIENTED_EDGE ( 'NONE', *, *, #17249, .F. ) ;
#17614 = CARTESIAN_POINT ( 'NONE',  ( 136.9873132030510305, -3657.938829547328169, 2239.009999999999764 ) ) ;
#17615 = ORIENTED_EDGE ( 'NONE', *, *, #11720, .F. ) ;
#17616 = VERTEX_POINT ( 'NONE', #13011 ) ;
#17617 = CARTESIAN_POINT ( 'NONE',  ( 4.918047856626605707, -3543.639179025994054, 2260.194362557658224 ) ) ;
#17618 = DATE_TIME_ROLE ( 'classification_date' ) ;
#17619 = FACE_OUTER_BOUND ( 'NONE', #3148, .T. ) ;
#17620 = DIRECTION ( 'NONE',  ( 1.000000000000000000, 0.000000000000000000, 0.000000000000000000 ) ) ;
#17621 = EDGE_LOOP ( 'NONE', ( #10977, #7482, #23064, #778, #8348 ) ) ;
#17622 = CIRCLE ( 'NONE', #13505, 1.269999999999882334 ) ;
#17623 = PLANE ( 'NONE',  #14457 ) ;
#17624 = FACE_BOUND ( 'NONE', #19063, .T. ) ;
#17625 = DIRECTION ( 'NONE',  ( 1.000000000000000000, 0.000000000000000000, 0.000000000000000000 ) ) ;
#17626 = DIRECTION ( 'NONE',  ( 0.000000000000000000, 0.000000000000000000, 1.000000000000000000 ) ) ;
#17627 = ORIENTED_EDGE ( 'NONE', *, *, #14881, .F. ) ;
#17628 = PERSON_AND_ORGANIZATION_ROLE ( 'creator' ) ;
#17629 = ORIENTED_EDGE ( 'NONE', *, *, #10371, .F. ) ;
#17630 = CARTESIAN_POINT ( 'NONE',  ( 12.70000000000000107, -3590.289999999999964, 2279.817639999999756 ) ) ;
#17631 = CARTESIAN_POINT ( 'NONE',  ( 10.32891780134183612, -3581.066905197333199, 2249.187322304957434 ) ) ;
#17632 = DIRECTION ( 'NONE',  ( 0.000000000000000000, 1.000000000000000000, -1.224646799147353207E-16 ) ) ;
#17633 = ORIENTED_EDGE ( 'NONE', *, *, #15866, .T. ) ;
#17634 = B_SPLINE_CURVE_WITH_KNOTS ( 'NONE', 3,
 ( #3884, #11033, #601, #18181, #7517, #14671, #21815, #9621, #816, #13133, #20620, #4688, #13475, #1053, #4570, #22373, #1161, #2812, #20288, #713, #13366, #15016, #11714, #13244, #20740, #16985, #15128, #7867, #6459, #18638, #4348, #6346, #4233, #9958, #22487, #6234, #18866, #11594, #22257, #17106, #2584, #13600, #934, #20398, #18523, #22035, #7983, #16767, #11839, #5998, #2934, #8208, #9731, #2480, #17215, #18990, #2693, #10071, #15355, #14907, #11372, #16873, #22145, #18746, #6118, #20508, #11487 ),
 .UNSPECIFIED., .F., .F.,
 ( 4, 2, 2, 2, 2, 2, 1, 1, 2, 2, 2, 2, 1, 1, 1, 2, 2, 2, 2, 1, 2, 2, 2, 2, 1, 1, 2, 2, 2, 2, 1, 2, 2, 2, 1, 1, 2, 2, 4 ),
 ( 0.000000000000000000, 0.06250000000155657431, 0.09375000000233692232, 0.1250000000031172565, 0.2500000000069327877, 0.3125000000086731733, 0.3437500000095414232, 0.3593750000100068842, 0.3671875000102372555, 0.3750000000104676823, 0.4375000000137948541, 0.4687500000154145030, 0.4843750000161757274, 0.4921875000165590319, 0.4960937500167533765, 0.4980468750169005920, 0.5000000000170478076, 0.5312500000163082881, 0.5468750000158427715, 0.5546875000155574442, 0.5585937500154427582, 0.5625000000153280721, 0.5937500000142669210, 0.6093750000137334588, 0.6171875000135523814, 0.6210937500136807232, 0.6230468750136081146, 0.6250000000135353950, 0.6875000000106663567, 0.7187500000092291730, 0.7343750000084173779, 0.7421875000081177287, 0.7500000000078179685, 0.8125000000061641803, 0.8437500000053371751, 0.8593750000049256155, 0.8671875000047818416, 0.8750000000046379567, 1.000000000000000000 ),
 .UNSPECIFIED. ) ;
#17635 = AXIS2_PLACEMENT_3D ( 'NONE', #4985, #15534, #1581 ) ;
#17636 = PLANE ( 'NONE',  #9951 ) ;
#17637 = AXIS2_PLACEMENT_3D ( 'NONE', #3523, #7172, #21807 ) ;
#17638 = DIRECTION ( 'NONE',  ( 0.000000000000000000, 1.000000000000000000, 0.000000000000000000 ) ) ;
#17639 = CARTESIAN_POINT ( 'NONE',  ( 145.0383630478528403, -3577.416324816570523, 2244.919872096889776 ) ) ;
#17640 = CARTESIAN_POINT ( 'NONE',  ( 12.69999999999999929, -3639.502500000000055, 2296.210799999999836 ) ) ;
#17641 = CARTESIAN_POINT ( 'NONE',  ( 11.81573155947770992, -3662.209820030859191, 2249.343846417981240 ) ) ;
#17642 = CARTESIAN_POINT ( 'NONE',  ( 12.69999999999999929, -3659.504999999999654, 2239.771999999999935 ) ) ;
#17643 = ORIENTED_EDGE ( 'NONE', *, *, #8936, .F. ) ;
#17644 = CARTESIAN_POINT ( 'NONE',  ( 63.50000000000000000, -3644.899999999999636, 2259.837999999999738 ) ) ;
#17645 = FACE_OUTER_BOUND ( 'NONE', #9725, .T. ) ;
#17646 = APPROVAL ( #8588, 'UNSPECIFIED' ) ;
#17647 = CYLINDRICAL_SURFACE ( 'NONE', #721, 11.11249999999985860 ) ;
#17648 = CARTESIAN_POINT ( 'NONE',  ( 14.61004568054142005, -3657.396752578035830, 2248.145630951006297 ) ) ;
#17649 = CARTESIAN_POINT ( 'NONE',  ( 22.55520000000100111, -3619.500000000000000, 2261.869999999999891 ) ) ;
#17650 = DIRECTION ( 'NONE',  ( 1.479750996568279710E-14, 0.000000000000000000, 1.000000000000000000 ) ) ;
#17651 = ORIENTED_EDGE ( 'NONE', *, *, #3973, .T. ) ;
#17652 = AXIS2_PLACEMENT_3D ( 'NONE', #9616, #20283, #16762 ) ;
#17653 = EDGE_CURVE ( 'NONE', #5562, #15820, #21909, .T. ) ;
#17654 = CARTESIAN_POINT ( 'NONE',  ( 139.6999999999999886, -3579.494999999999891, 2244.978999999999814 ) ) ;
#17655 = EDGE_CURVE ( 'NONE', #12971, #14270, #4505, .T. ) ;
#17656 = DIRECTION ( 'NONE',  ( -1.000000000000000000, -0.000000000000000000, -0.000000000000000000 ) ) ;
#17657 = SECURITY_CLASSIFICATION_LEVEL ( 'unclassified' ) ;
#17658 = EDGE_CURVE ( 'NONE', #14926, #14558, #8422, .T. ) ;
#17659 = DIRECTION ( 'NONE',  ( 0.8660254037840939834, -0.5000000000005969669, 0.000000000000000000 ) ) ;
#17660 = CARTESIAN_POINT ( 'NONE',  ( 25.39999999999999858, -3568.700000000000273, 2260.600000000000364 ) ) ;
#17661 = CARTESIAN_POINT ( 'NONE',  ( 12.69999999999999929, -3599.497499999999945, 2296.591799999999694 ) ) ;
#17662 = AXIS2_PLACEMENT_3D ( 'NONE', #5692, #7332, #16452 ) ;
#17663 = CARTESIAN_POINT ( 'NONE',  ( 127.0000000000000000, -3670.300000000000182, 2260.600000000000364 ) ) ;
#17664 = DIRECTION ( 'NONE',  ( 1.000000000000000000, 0.000000000000000000, 0.000000000000000000 ) ) ;
#17665 = EDGE_CURVE ( 'NONE', #14593, #16647, #16576, .T. ) ;
#17666 = VECTOR ( 'NONE', #7755, 1000.000000000000000 ) ;
#17667 = CARTESIAN_POINT ( 'NONE',  ( 139.6999999999999886, -3659.504999999999654, 2246.630000000000109 ) ) ;
#17668 = EDGE_LOOP ( 'NONE', ( #6084, #8602, #11953, #11194 ) ) ;
#17669 = DIRECTION ( 'NONE',  ( 1.000000000000000000, 0.000000000000000000, 0.000000000000000000 ) ) ;
#17670 = AXIS2_PLACEMENT_3D ( 'NONE', #2899, #1129, #3125 ) ;
#17671 = DIRECTION ( 'NONE',  ( 0.000000000000000000, 2.336881798971000105E-14, 1.000000000000000000 ) ) ;
#17672 = ORIENTED_EDGE ( 'NONE', *, *, #22539, .T. ) ;
#17673 = ADVANCED_FACE ( 'NONE', ( #14769 ), #6487, .T. ) ;
#17674 = DIRECTION ( 'NONE',  ( 1.000000000000000000, 0.000000000000000000, 0.000000000000000000 ) ) ;
#17675 = ORIENTED_EDGE ( 'NONE', *, *, #13501, .T. ) ;
#17676 = CARTESIAN_POINT ( 'NONE',  ( 114.2999999999999972, -3644.899999999999636, 2239.009999999999764 ) ) ;
#17677 = VECTOR ( 'NONE', #15050, 1000.000000000000000 ) ;
#17678 = ORIENTED_EDGE ( 'NONE', *, *, #12718, .T. ) ;
#17679 = ORIENTED_EDGE ( 'NONE', *, *, #2702, .T. ) ;
#17680 = COORDINATED_UNIVERSAL_TIME_OFFSET ( 0, 0, .AHEAD. ) ;
#17681 = FACE_OUTER_BOUND ( 'NONE', #21287, .T. ) ;
#17682 = ORIENTED_EDGE ( 'NONE', *, *, #6579, .T. ) ;
#17684 = CARTESIAN_POINT ( 'NONE',  ( 145.4009155966692788, -3579.898563401719002, 2244.742832167291454 ) ) ;
#17683 = TOROIDAL_SURFACE ( 'NONE', #19202, 3.606799999998999695, 0.7620000000000000107 ) ;
#17685 = EDGE_CURVE ( 'NONE', #21948, #13787, #19213, .T. ) ;
#17686 = APPROVAL_STATUS ( 'not_yet_approved' ) ;
#17687 = EDGE_CURVE ( 'NONE', #11834, #11029, #9117, .T. ) ;
#17688 = CIRCLE ( 'NONE', #5359, 11.11250000000000071 ) ;
#17689 = DIRECTION ( 'NONE',  ( 0.000000000000000000, 0.000000000000000000, 1.000000000000000000 ) ) ;
#17690 = B_SPLINE_CURVE_WITH_KNOTS ( 'NONE', 3,
 ( #16413, #3646, #17936, #5770, #16526, #19824, #366, #12557, #10911, #10796, #12900, #12440, #5541, #18059, #2132, #7510, #19713, #14666, #16188 ),
 .UNSPECIFIED., .F., .F.,
 ( 4, 1, 1, 1, 1, 1, 1, 1, 1, 1, 1, 1, 1, 1, 1, 1, 4 ),
 ( 0.000000000000000000, 0.06250000000000000000, 0.1250000000000000000, 0.1875000000000000000, 0.2500000000000000000, 0.3125000000000000000, 0.3750000000000000000, 0.4375000000000000000, 0.5000000000000000000, 0.5625000000000000000, 0.6250000000000000000, 0.6875000000000000000, 0.7500000000000000000, 0.8125000000000000000, 0.8750000000000000000, 0.9375000000000000000, 0.9999968116805088014 ),
 .UNSPECIFIED. ) ;
#17691 = CARTESIAN_POINT ( 'NONE',  ( 9.525000000092171959, -3544.061999999999898, 2281.351800000095409 ) ) ;
#17692 = CARTESIAN_POINT ( 'NONE',  ( 95.25000000000000000, -3568.700000000000273, 2244.547199999999975 ) ) ;
#17693 = DIRECTION ( 'NONE',  ( 0.000000000000000000, 0.000000000000000000, -1.000000000000000000 ) ) ;
#17694 = LINE ( 'NONE', #22844, #19243 ) ;
#17695 = EDGE_LOOP ( 'NONE', ( #11305, #4303, #19089, #16467 ) ) ;
#17696 = AXIS2_PLACEMENT_3D ( 'NONE', #2912, #10170, #15223 ) ;
#17697 = CARTESIAN_POINT ( 'NONE',  ( 15.54902373130514981, -3695.599092773423763, 2255.000110291663077 ) ) ;
#17698 = CARTESIAN_POINT ( 'NONE',  ( 28.24479999999899604, -3568.700000000000273, 2261.869999999999891 ) ) ;
#17699 = ORIENTED_EDGE ( 'NONE', *, *, #20969, .F. ) ;
#17700 = CARTESIAN_POINT ( 'NONE',  ( 4.909231720582250880, -3695.380630526287405, 2260.172378166327235 ) ) ;
#17701 = DIRECTION ( 'NONE',  ( 0.000000000000000000, -1.000000000000000000, 0.000000000000000000 ) ) ;
#17702 = CIRCLE ( 'NONE', #18818, 3.175000000000149925 ) ;
#17703 = DIRECTION ( 'NONE',  ( 0.5000000000043351989, -0.8660254037819355988, 0.000000000000000000 ) ) ;
#17704 = ORIENTED_EDGE ( 'NONE', *, *, #12109, .T. ) ;
#17705 = DIRECTION ( 'NONE',  ( 0.000000000000000000, 0.000000000000000000, -1.000000000000000000 ) ) ;
#17706 = CARTESIAN_POINT ( 'NONE',  ( 95.25000000000000000, -3694.430000000000291, 2250.236800000000130 ) ) ;
#17707 = ORIENTED_EDGE ( 'NONE', *, *, #19387, .F. ) ;
#17708 = CYLINDRICAL_SURFACE ( 'NONE', #3470, 2.844799999998998796 ) ;
#17709 = FACE_OUTER_BOUND ( 'NONE', #16291, .T. ) ;
#17710 = EDGE_CURVE ( 'NONE', #13716, #20178, #17286, .T. ) ;
#17711 = CARTESIAN_POINT ( 'NONE',  ( 136.8551999999999964, -3579.425093798000034, 2250.181036214999949 ) ) ;
#17712 = AXIS2_PLACEMENT_3D ( 'NONE', #13651, #10246, #3531 ) ;
#17713 = APPLICATION_PROTOCOL_DEFINITION ( 'international standard', 'automotive_design', 2000, #3350 ) ;
#17714 = CIRCLE ( 'NONE', #19976, 0.7619999999999294005 ) ;
#17715 = DIRECTION ( 'NONE',  ( 1.000000000000000000, 0.000000000000000000, 0.000000000000000000 ) ) ;
#17716 = PLANE ( 'NONE',  #18784 ) ;
#17717 = DIRECTION ( 'NONE',  ( 0.000000000000000000, -1.000000000000000000, 0.000000000000000000 ) ) ;
#17718 = EDGE_CURVE ( 'NONE', #724, #14116, #1605, .T. ) ;
#17719 = AXIS2_PLACEMENT_3D ( 'NONE', #8316, #1039, #8664 ) ;
#17720 = CARTESIAN_POINT ( 'NONE',  ( 137.1914968215908459, -3658.160756285533807, 2249.438291734014911 ) ) ;
#17721 = EDGE_CURVE ( 'NONE', #21259, #6861, #2001, .T. ) ;
#17722 = EDGE_CURVE ( 'NONE', #2712, #2680, #10983, .T. ) ;
#17723 = ORIENTED_EDGE ( 'NONE', *, *, #20102, .T. ) ;
#17724 = CARTESIAN_POINT ( 'NONE',  ( 136.9601134096845385, -3660.284759461715112, 2250.236799783840979 ) ) ;
#17725 = VERTEX_POINT ( 'NONE', #22585 ) ;
#17726 = ORIENTED_EDGE ( 'NONE', *, *, #7848, .F. ) ;
#17727 = EDGE_CURVE ( 'NONE', #11029, #22409, #13978, .T. ) ;
#17728 = ORIENTED_EDGE ( 'NONE', *, *, #10647, .T. ) ;
#17729 = AXIS2_PLACEMENT_3D ( 'NONE', #16605, #1855, #554 ) ;
#17730 = AXIS2_PLACEMENT_3D ( 'NONE', #19625, #22891, #3567 ) ;
#17731 = DIRECTION ( 'NONE',  ( 1.000000000000000000, 5.432398939370942693E-28, -2.324635735433000053E-14 ) ) ;
#17732 = ORIENTED_EDGE ( 'NONE', *, *, #3973, .F. ) ;
#17733 = ORIENTED_EDGE ( 'NONE', *, *, #4511, .T. ) ;
#17734 = DIRECTION ( 'NONE',  ( 1.000000000000000000, 0.000000000000000000, 0.000000000000000000 ) ) ;
#17735 = COORDINATED_UNIVERSAL_TIME_OFFSET ( 0, 0, .AHEAD. ) ;
#17736 = DIRECTION ( 'NONE',  ( 0.000000000000000000, 0.000000000000000000, -1.000000000000000000 ) ) ;
#17737 = FACE_OUTER_BOUND ( 'NONE', #22724, .T. ) ;
#17738 = EDGE_CURVE ( 'NONE', #8260, #4017, #16936, .T. ) ;
#17739 = ORIENTED_EDGE ( 'NONE', *, *, #6312, .T. ) ;
#17740 = DIRECTION ( 'NONE',  ( 0.000000000000000000, -1.000000000000000000, 0.000000000000000000 ) ) ;
#17741 = EDGE_CURVE ( 'NONE', #17848, #671, #13346, .T. ) ;
#17742 = DIRECTION ( 'NONE',  ( 1.000000000000000000, 0.000000000000000000, 0.000000000000000000 ) ) ;
#17743 = DIRECTION ( 'NONE',  ( -1.000000000000000000, 0.000000000000000000, 0.000000000000000000 ) ) ;
#17744 = CARTESIAN_POINT ( 'NONE',  ( 50.79999999999999716, -3619.500000000000000, 2239.771999999999935 ) ) ;
#17745 = ORIENTED_EDGE ( 'NONE', *, *, #5815, .T. ) ;
#17746 = APPROVAL_ROLE ( '' ) ;
#17747 = ORIENTED_EDGE ( 'NONE', *, *, #9579, .T. ) ;
#17748 = CARTESIAN_POINT ( 'NONE',  ( 12.69999999996000106, -3602.629840905000037, 2296.591799999999694 ) ) ;
#17749 = TOROIDAL_SURFACE ( 'NONE', #20023, 5.080000000000000071, 0.3810000000000000053 ) ;
#17750 = AXIS2_PLACEMENT_3D ( 'NONE', #3960, #20140, #11115 ) ;
#17751 = DIRECTION ( 'NONE',  ( 0.000000000000000000, 0.000000000000000000, 1.000000000000000000 ) ) ;
#17752 = ADVANCED_FACE ( 'NONE', ( #15573 ), #2672, .T. ) ;
#17753 = ORIENTED_EDGE ( 'NONE', *, *, #6507, .F. ) ;
#17754 = FACE_OUTER_BOUND ( 'NONE', #8294, .T. ) ;
#17755 = CIRCLE ( 'NONE', #1660, 2.844800000000091700 ) ;
#17756 = ORIENTED_EDGE ( 'NONE', *, *, #11024, .T. ) ;
#17757 = DIRECTION ( 'NONE',  ( -2.061772070699084901E-14, 0.5000000000031208369, -0.8660254037826368156 ) ) ;
#17758 = CARTESIAN_POINT ( 'NONE',  ( 139.6999999999999886, -3659.504999999999654, 2270.760000000000218 ) ) ;
#17759 = CARTESIAN_POINT ( 'NONE',  ( 95.25000000000000000, -3670.300000000000182, 2250.236800000000130 ) ) ;
#17760 = FACE_OUTER_BOUND ( 'NONE', #23020, .T. ) ;
#17761 = CARTESIAN_POINT ( 'NONE',  ( 22.55520000000100111, -3619.500000000000000, 2259.837999999999738 ) ) ;
#17762 = CARTESIAN_POINT ( 'NONE',  ( 15.87500000000000000, -3544.061999999999898, 2281.351799999999912 ) ) ;
#17763 = EDGE_LOOP ( 'NONE', ( #13069, #7036, #3560, #12582, #12124, #10023 ) ) ;
#17764 = AXIS2_PLACEMENT_3D ( 'NONE', #8834, #19148, #11884 ) ;
#17765 = DIRECTION ( 'NONE',  ( 0.000000000000000000, 0.000000000000000000, -1.000000000000000000 ) ) ;
#17766 = VECTOR ( 'NONE', #19706, 1000.000000000000000 ) ;
#17767 = FACE_OUTER_BOUND ( 'NONE', #16337, .T. ) ;
#17768 = LINE ( 'NONE', #8758, #17545 ) ;
#17769 = TOROIDAL_SURFACE ( 'NONE', #17367, 3.606799999999999784, 0.7620000000000000107 ) ;
#17770 = CARTESIAN_POINT ( 'NONE',  ( 15.33227593808441469, -3658.426079296531043, 2249.662570456160665 ) ) ;
#17771 = CARTESIAN_POINT ( 'NONE',  ( 136.8326572973758744, -3695.618941226884999, 2254.954211613487587 ) ) ;
#17772 = EDGE_LOOP ( 'NONE', ( #14532, #7319, #5684, #335 ) ) ;
#17773 = CARTESIAN_POINT ( 'NONE',  ( 10.45084209371125183, -3577.751058544115040, 2250.012766604421813 ) ) ;
#17774 = ORIENTED_EDGE ( 'NONE', *, *, #9968, .F. ) ;
#17775 = CARTESIAN_POINT ( 'NONE',  ( 139.6999999997610757, -3582.627340905411984, 2239.009999999999764 ) ) ;
#17776 = CARTESIAN_POINT ( 'NONE',  ( 15.41268679705191857, -3661.071170452636579, 2239.009999999999764 ) ) ;
#17777 = COORDINATED_UNIVERSAL_TIME_OFFSET ( 0, 0, .AHEAD. ) ;
#17778 = CARTESIAN_POINT ( 'NONE',  ( 15.87500000000000000, -3544.061999999999898, 2281.351799999999912 ) ) ;
#17779 = DIRECTION ( 'NONE',  ( -1.000000000000000000, 0.000000000000000000, 0.000000000000000000 ) ) ;
#17780 = DIRECTION ( 'NONE',  ( 1.000000000000000000, 0.000000000000000000, 0.000000000000000000 ) ) ;
#17781 = CIRCLE ( 'NONE', #14797, 3.175000000000149925 ) ;
#17782 = VECTOR ( 'NONE', #17089, 1000.000000000000114 ) ;
#17783 = DIRECTION ( 'NONE',  ( 1.000000000000000000, -0.000000000000000000, -0.000000000000000000 ) ) ;
#17784 = APPLIED_PERSON_AND_ORGANIZATION_ASSIGNMENT ( #14302, #14417, ( #22639 ) ) ;
#17785 = CIRCLE ( 'NONE', #2074, 0.3809999999999647002 ) ;
#17786 = AXIS2_PLACEMENT_3D ( 'NONE', #726, #15038, #624 ) ;
#17787 = ORIENTED_EDGE ( 'NONE', *, *, #1628, .F. ) ;
#17788 = DIRECTION ( 'NONE',  ( 0.000000000000000000, -1.000000000000000000, 0.000000000000000000 ) ) ;
#17789 = VERTEX_POINT ( 'NONE', #22468 ) ;
#17790 = DIRECTION ( 'NONE',  ( -1.000000000000000000, 0.000000000000000000, 0.000000000000000000 ) ) ;
#17791 = ADVANCED_FACE ( 'NONE', ( #8075 ), #1260, .F. ) ;
#17792 = DIRECTION ( 'NONE',  ( 2.324635735433000053E-14, 0.000000000000000000, 1.000000000000000000 ) ) ;
#17793 = ORIENTED_EDGE ( 'NONE', *, *, #13807, .F. ) ;
#17794 = LINE ( 'NONE', #8898, #6558 ) ;
#17795 = EDGE_CURVE ( 'NONE', #8900, #13472, #22557, .T. ) ;
#17796 = ORIENTED_EDGE ( 'NONE', *, *, #5241, .T. ) ;
#17797 = FACE_OUTER_BOUND ( 'NONE', #20606, .T. ) ;
#17798 = CARTESIAN_POINT ( 'NONE',  ( 139.6999999999999886, -3579.494999999999891, 2270.760000000000218 ) ) ;
#17799 = CIRCLE ( 'NONE', #2819, 1.270000000000000018 ) ;
#17800 = AXIS2_PLACEMENT_3D ( 'NONE', #18254, #21664, #21997 ) ;
#17801 = EDGE_LOOP ( 'NONE', ( #12851, #3497 ) ) ;
#17802 = ORIENTED_EDGE ( 'NONE', *, *, #2364, .T. ) ;
#17803 = AXIS2_PLACEMENT_3D ( 'NONE', #7958, #16746, #4325 ) ;
#17804 = CARTESIAN_POINT ( 'NONE',  ( 136.9377862181021897, -3580.181062415173074, 2249.913373991909793 ) ) ;
#17805 = VERTEX_POINT ( 'NONE', #3141 ) ;
#17806 = CARTESIAN_POINT ( 'NONE',  ( 116.8400000000000034, -3695.699999999999818, 2247.392000000000280 ) ) ;
#17807 = DATE_AND_TIME ( #12537, #22092 ) ;
#17808 = CARTESIAN_POINT ( 'NONE',  ( 142.0316867972038608, -3660.851200000135123, 2239.167815367293770 ) ) ;
#17809 = DIRECTION ( 'NONE',  ( 0.000000000000000000, 0.000000000000000000, 1.000000000000000000 ) ) ;
#17810 = LINE ( 'NONE', #17692, #16026 ) ;
#17811 = APPROVAL ( #21650, 'UNSPECIFIED' ) ;
#17812 = DIRECTION ( 'NONE',  ( 0.000000000000000000, -1.000000000000000000, 0.000000000000000000 ) ) ;
#17813 = B_SPLINE_CURVE_WITH_KNOTS ( 'NONE', 3,
 ( #19469, #1777, #3411, #14204, #21350, #16068 ),
 .UNSPECIFIED., .F., .F.,
 ( 4, 1, 1, 4 ),
 ( 0.000000000000000000, 0.3333333333333000081, 0.6666666666667000474, 1.000000000000000000 ),
 .UNSPECIFIED. ) ;
#17814 = CIRCLE ( 'NONE', #7719, 3.606799999998994366 ) ;
#17815 = LINE ( 'NONE', #1768, #20704 ) ;
#17816 = ORIENTED_EDGE ( 'NONE', *, *, #3765, .F. ) ;
#17817 = AXIS2_PLACEMENT_3D ( 'NONE', #7909, #13068, #20443 ) ;
#17818 = DIRECTION ( 'NONE',  ( 1.000000000000000000, 0.000000000000000000, 0.000000000000000000 ) ) ;
#17819 = AXIS2_PLACEMENT_3D ( 'NONE', #9824, #9938, #15340 ) ;
#17820 = EDGE_CURVE ( 'NONE', #7575, #16167, #8728, .T. ) ;
#17821 = CARTESIAN_POINT ( 'NONE',  ( 138.3436566013999993, -3577.145744321000166, 2239.391000000000076 ) ) ;
#17822 = ORIENTED_EDGE ( 'NONE', *, *, #18398, .T. ) ;
#17823 = DIRECTION ( 'NONE',  ( 1.000000000000000000, 0.000000000000000000, 0.000000000000000000 ) ) ;
#17824 = DIRECTION ( 'NONE',  ( 0.000000000000000000, 1.000000000000000000, 0.000000000000000000 ) ) ;
#17825 = AXIS2_PLACEMENT_3D ( 'NONE', #12610, #16234, #7219 ) ;
#17826 = ADVANCED_FACE ( 'NONE', ( #3024 ), #1143, .F. ) ;
#17827 = DIRECTION ( 'NONE',  ( 0.000000000000000000, 0.000000000000000000, -1.000000000000000000 ) ) ;
#17828 = CIRCLE ( 'NONE', #1361, 0.7619999999999294005 ) ;
#17829 = VERTEX_POINT ( 'NONE', #6680 ) ;
#17830 = CARTESIAN_POINT ( 'NONE',  ( 0.7620000000000000107, -3695.699999999999818, 2295.829799999999977 ) ) ;
#17831 = FACE_OUTER_BOUND ( 'NONE', #23113, .T. ) ;
#17832 = ORIENTED_EDGE ( 'NONE', *, *, #9300, .T. ) ;
#17833 = CARTESIAN_POINT ( 'NONE',  ( 47.95519999999999783, -3619.500000000000000, 2259.837999999999738 ) ) ;
#17834 = DIRECTION ( 'NONE',  ( 0.000000000000000000, -1.000000000000000000, 0.000000000000000000 ) ) ;
#17835 = LINE ( 'NONE', #1219, #15479 ) ;
#17836 = EDGE_CURVE ( 'NONE', #13352, #21090, #2375, .T. ) ;
#17837 = UNCERTAINTY_MEASURE_WITH_UNIT (LENGTH_MEASURE( 1.000000000000000082E-05 ), #13621, 'distance_accuracy_value', 'NONE');
#17838 = CARTESIAN_POINT ( 'NONE',  ( 25.39999999999999858, -3578.860000000000127, 2247.392000000000280 ) ) ;
#17839 = PERSON_AND_ORGANIZATION ( #5446, #1895 ) ;
#17840 = CIRCLE ( 'NONE', #16712, 3.606800000000000228 ) ;
#17841 = CARTESIAN_POINT ( 'NONE',  ( 15.41268679713999923, -3599.497499999999945, 2296.210799999999836 ) ) ;
#17842 = CARTESIAN_POINT ( 'NONE',  ( 139.6999999999999886, -3654.043999999999869, 2245.359999999999673 ) ) ;
#17843 = ORIENTED_EDGE ( 'NONE', *, *, #21897, .F. ) ;
#17844 = CYLINDRICAL_SURFACE ( 'NONE', #13402, 2.844799999998998796 ) ;
#17845 = EDGE_CURVE ( 'NONE', #13123, #309, #7598, .T. ) ;
#17846 = AXIS2_PLACEMENT_3D ( 'NONE', #18501, #16850, #18271 ) ;
#17847 = CARTESIAN_POINT ( 'NONE',  ( 137.2921315476570499, -3657.990157942962924, 2249.255081503176370 ) ) ;
#17848 = VERTEX_POINT ( 'NONE', #13580 ) ;
#17849 = ORIENTED_EDGE ( 'NONE', *, *, #5818, .F. ) ;
#17850 = ORIENTED_EDGE ( 'NONE', *, *, #3359, .T. ) ;
#17851 = VERTEX_POINT ( 'NONE', #22353 ) ;
#17852 = ADVANCED_FACE ( 'NONE', ( #17432 ), #4665, .T. ) ;
#17853 = CARTESIAN_POINT ( 'NONE',  ( 145.4149999999999920, -3659.504999999999654, 2246.630000000000109 ) ) ;
#17854 = EDGE_LOOP ( 'NONE', ( #16499, #2695, #16250, #9576 ) ) ;
#17855 = ORIENTED_EDGE ( 'NONE', *, *, #8889, .T. ) ;
#17856 = CARTESIAN_POINT ( 'NONE',  ( 5.080000000000000071, -3544.570000000000164, 2260.600000000000364 ) ) ;
#17857 = ITEM_DEFINED_TRANSFORMATION ( 'NONE', 'NONE', #7874,  #5611 ) ;
#17858 = FACE_OUTER_BOUND ( 'NONE', #12158, .T. ) ;
#17859 = CARTESIAN_POINT ( 'NONE',  ( 9.855200000000998273, -3659.504999999999654, 2256.063560000000052 ) ) ;
#17860 = EDGE_CURVE ( 'NONE', #4945, #18837, #9848, .T. ) ;
#17861 = ORIENTED_EDGE ( 'NONE', *, *, #22098, .T. ) ;
#17862 = AXIS2_PLACEMENT_3D ( 'NONE', #11216, #16379, #7473 ) ;
#17863 = EDGE_CURVE ( 'NONE', #16691, #3271, #149, .T. ) ;
#17864 = CARTESIAN_POINT ( 'NONE',  ( 57.14999999999969305, -3670.300000000000182, 2244.547199999999975 ) ) ;
#17865 = VERTEX_POINT ( 'NONE', #8190 ) ;
#17866 = CIRCLE ( 'NONE', #1395, 1.269999999999882334 ) ;
#17867 = DIRECTION ( 'NONE',  ( 1.000000000000000000, 0.000000000000000000, 0.000000000000000000 ) ) ;
#17868 = DIRECTION ( 'NONE',  ( 0.000000000000000000, 0.000000000000000000, -1.000000000000000000 ) ) ;
#17869 = LINE ( 'NONE', #10835, #7438 ) ;
#17870 = DATE_AND_TIME ( #14243, #4905 ) ;
#17871 = CARTESIAN_POINT ( 'NONE',  ( 131.8392664897742179, -3543.487248044008538, 2259.997203529242142 ) ) ;
#17872 = DIRECTION ( 'NONE',  ( 1.000000000000000000, 0.000000000000000000, 0.000000000000000000 ) ) ;
#17873 = AXIS2_PLACEMENT_3D ( 'NONE', #12883, #348, #19803 ) ;
#17874 = VERTEX_POINT ( 'NONE', #15336 ) ;
#17875 = CYLINDRICAL_SURFACE ( 'NONE', #9699, 2.844800000000091700 ) ;
#17876 = ORIENTED_EDGE ( 'NONE', *, *, #23160, .T. ) ;
#17877 = ADVANCED_FACE ( 'NONE', ( #11816 ), #15452, .T. ) ;
#17878 = FACE_BOUND ( 'NONE', #12804, .T. ) ;
#17879 = AXIS2_PLACEMENT_3D ( 'NONE', #10781, #12770, #9 ) ;
#17880 = CARTESIAN_POINT ( 'NONE',  ( -12.31900000000003459, -3581.552400000169200, 2247.392000000001190 ) ) ;
#17881 = DIRECTION ( 'NONE',  ( 1.000000000000000000, 0.000000000000000000, 0.000000000000000000 ) ) ;
#17882 = CARTESIAN_POINT ( 'NONE',  ( 12.69999999999999929, -3648.710000000000036, 2275.055139999999483 ) ) ;
#17883 = DIRECTION ( 'NONE',  ( 0.000000000000000000, 0.000000000000000000, -1.000000000000000000 ) ) ;
#17884 = VERTEX_POINT ( 'NONE', #19989 ) ;
#17885 = CARTESIAN_POINT ( 'NONE',  ( 18.23925622610050823, -3658.098689426352394, 2245.410334305951437 ) ) ;
#17886 = ORIENTED_EDGE ( 'NONE', *, *, #19022, .F. ) ;
#17887 = CYLINDRICAL_SURFACE ( 'NONE', #891, 0.3810000000000330345 ) ;
#17888 = CARTESIAN_POINT ( 'NONE',  ( -0.7620000000000000107, -3694.938000000000102, 2253.487999999999829 ) ) ;
#17889 = AXIS2_PLACEMENT_3D ( 'NONE', #11517, #965, #2723 ) ;
#17890 = EDGE_CURVE ( 'NONE', #10620, #5839, #12402, .T. ) ;
#17891 = CARTESIAN_POINT ( 'NONE',  ( 139.6999999999999886, -3570.287499999999909, 2268.705139999999574 ) ) ;
#17892 = CARTESIAN_POINT ( 'NONE',  ( 14.63011727138534646, -3657.415010725946104, 2248.209217256212014 ) ) ;
#17893 = LINE ( 'NONE', #17649, #18427 ) ;
#17894 = EDGE_LOOP ( 'NONE', ( #22406, #738, #3554, #21888 ) ) ;
#17895 = DIRECTION ( 'NONE',  ( -1.000000000000000000, 0.000000000000000000, 0.000000000000000000 ) ) ;
#17896 = ORIENTED_EDGE ( 'NONE', *, *, #11212, .F. ) ;
#17897 = DIRECTION ( 'NONE',  ( 1.000000000000000000, 0.000000000000000000, 0.000000000000000000 ) ) ;
#17898 = LINE ( 'NONE', #5368, #14522 ) ;
#17899 = COORDINATED_UNIVERSAL_TIME_OFFSET ( 0, 0, .AHEAD. ) ;
#17900 = CARTESIAN_POINT ( 'NONE',  ( 0.000000000000000000, -3694.430000000000291, 2259.329999999999927 ) ) ;
#17901 = DIRECTION ( 'NONE',  ( -1.224646799147353207E-16, 1.000000000000000000, 0.000000000000000000 ) ) ;
#17902 = DIRECTION ( 'NONE',  ( 1.224646799147353207E-16, 1.000000000000000000, -0.000000000000000000 ) ) ;
#17903 = EDGE_CURVE ( 'NONE', #6114, #15102, #12112, .T. ) ;
#17904 = CARTESIAN_POINT ( 'NONE',  ( 15.74707948048999917, -3543.299999999999727, 2254.503999999999905 ) ) ;
#17905 = VERTEX_POINT ( 'NONE', #9207 ) ;
#17906 = LINE ( 'NONE', #14631, #11736 ) ;
#17907 = ORIENTED_EDGE ( 'NONE', *, *, #21537, .T. ) ;
#17908 = DIRECTION ( 'NONE',  ( 0.000000000000000000, 0.000000000000000000, -1.000000000000000000 ) ) ;
#17909 = DIRECTION ( 'NONE',  ( 0.000000000000000000, -1.000000000000000000, 0.000000000000000000 ) ) ;
#17910 = EDGE_LOOP ( 'NONE', ( #6856, #11635, #1480, #15030 ) ) ;
#17911 = CYLINDRICAL_SURFACE ( 'NONE', #22252, 2.844799999998998796 ) ;
#17912 = ORIENTED_EDGE ( 'NONE', *, *, #12293, .F. ) ;
#17913 = DIRECTION ( 'NONE',  ( 0.000000000000000000, 0.000000000000000000, -1.000000000000000000 ) ) ;
#17914 = ORIENTED_EDGE ( 'NONE', *, *, #17471, .T. ) ;
#17915 = APPLIED_PERSON_AND_ORGANIZATION_ASSIGNMENT ( #8647, #3480, ( #43 ) ) ;
#17916 = CARTESIAN_POINT ( 'NONE',  ( 137.0191252110892322, -3580.447152269891376, 2249.753138802207559 ) ) ;
#17917 = VERTEX_POINT ( 'NONE', #1611 ) ;
#17918 = DIRECTION ( 'NONE',  ( 0.000000000000000000, 0.000000000000000000, -1.000000000000000000 ) ) ;
#17919 = PERSON_AND_ORGANIZATION ( #5446, #1895 ) ;
#17920 = CARTESIAN_POINT ( 'NONE',  ( 117.1447999999989946, -3594.099999999999909, 2261.869999999999891 ) ) ;
#17921 = DIRECTION ( 'NONE',  ( 0.000000000000000000, 1.000000000000000000, 0.000000000000000000 ) ) ;
#17922 = CARTESIAN_POINT ( 'NONE',  ( 10.16000000000000014, -3580.776127254000130, 2255.774000000000342 ) ) ;
#17923 = DIRECTION ( 'NONE',  ( -1.000000000000000000, 0.000000000000000000, 0.000000000000000000 ) ) ;
#17924 = CARTESIAN_POINT ( 'NONE',  ( 140.7110437557817590, -3576.835571923886619, 2249.390760484202474 ) ) ;
#17925 = EDGE_LOOP ( 'NONE', ( #7031, #14691, #17527, #161 ) ) ;
#17926 = CARTESIAN_POINT ( 'NONE',  ( 5.080000000000000071, -3544.570000000000164, 2260.600000000000364 ) ) ;
#17927 = AXIS2_PLACEMENT_3D ( 'NONE', #7102, #6993, #8970 ) ;
#17928 = ORIENTED_EDGE ( 'NONE', *, *, #18110, .F. ) ;
#17929 = DIRECTION ( 'NONE',  ( 0.000000000000000000, 1.000000000000000000, 0.000000000000000000 ) ) ;
#17930 = EDGE_LOOP ( 'NONE', ( #12603, #16935, #23004, #6134 ) ) ;
#17931 = CARTESIAN_POINT ( 'NONE',  ( 4.771243568379631483, -3695.598810868119926, 2259.826779105117112 ) ) ;
#17932 = AXIS2_PLACEMENT_3D ( 'NONE', #16472, #428, #16703 ) ;
#17933 = LINE ( 'NONE', #14435, #21848 ) ;
#17934 = DIRECTION ( 'NONE',  ( 1.000000000000000000, 0.000000000000000000, 0.000000000000000000 ) ) ;
#17935 = ORIENTED_EDGE ( 'NONE', *, *, #14142, .F. ) ;
#17936 = CARTESIAN_POINT ( 'NONE',  ( 12.97541421502999981, -3662.340907203999905, 2257.594921553999939 ) ) ;
#17937 = DIRECTION ( 'NONE',  ( -2.903809793931999834E-13, 4.457650181899999573E-12, 1.000000000000000000 ) ) ;
#17938 = ORIENTED_EDGE ( 'NONE', *, *, #21642, .F. ) ;
#17939 = APPLIED_PERSON_AND_ORGANIZATION_ASSIGNMENT ( #733, #16901, ( #16085 ) ) ;
#17940 = CARTESIAN_POINT ( 'NONE',  ( 12.69999999999999929, -3653.789999999999964, 2263.117139999999836 ) ) ;
#17941 = CARTESIAN_POINT ( 'NONE',  ( 152.4000000000000057, -3695.699999999999818, 2296.591799999999694 ) ) ;
#17942 =( LENGTH_UNIT ( ) NAMED_UNIT ( * ) SI_UNIT ( .MILLI., .METRE. ) );
#17943 = DIRECTION ( 'NONE',  ( 0.000000000000000000, 0.000000000000000000, -1.000000000000000000 ) ) ;
#17944 = CYLINDRICAL_SURFACE ( 'NONE', #19735, 2.844800000000001550 ) ;
#17945 = APPROVAL_DATE_TIME ( #7071, #10348 ) ;
#17946 = EDGE_LOOP ( 'NONE', ( #2820, #3537, #22078, #13306 ) ) ;
#17947 = TOROIDAL_SURFACE ( 'NONE', #10487, 3.606799999999999784, 0.7620000000000000107 ) ;
#17948 = ADVANCED_FACE ( 'NONE', ( #16349 ), #4255, .T. ) ;
#17949 = LINE ( 'NONE', #12567, #13017 ) ;
#17950 = DIRECTION ( 'NONE',  ( 0.000000000000000000, 1.000000000000000000, 0.000000000000000000 ) ) ;
#17951 = EDGE_LOOP ( 'NONE', ( #20991, #11122, #19564, #20305, #23059, #12020 ) ) ;
#17952 = APPLIED_APPROVAL_ASSIGNMENT ( #5337, ( #4122 ) ) ;
#17954 = EDGE_CURVE ( 'NONE', #23086, #20690, #10234, .T. ) ;
#17953 = CARTESIAN_POINT ( 'NONE',  ( 18.27191195451976569, -3580.765843483243316, 2245.279837209925972 ) ) ;
#17955 = CIRCLE ( 'NONE', #20205, 3.606799999999001027 ) ;
#17956 = ADVANCED_FACE ( 'NONE', ( #15922, #2178 ), #10526, .T. ) ;
#17957 = DIRECTION ( 'NONE',  ( 0.000000000000000000, 0.000000000000000000, 1.000000000000000000 ) ) ;
#17958 = EDGE_LOOP ( 'NONE', ( #1031, #20365, #19198, #12818 ) ) ;
#17959 = VERTEX_POINT ( 'NONE', #23053 ) ;
#17960 = CARTESIAN_POINT ( 'NONE',  ( 137.1966912320340271, -3660.857380486106194, 2250.145240675303285 ) ) ;
#17961 = ORIENTED_EDGE ( 'NONE', *, *, #1621, .F. ) ;
#17962 = VERTEX_POINT ( 'NONE', #304 ) ;
#17963 = EDGE_CURVE ( 'NONE', #22650, #4556, #20349, .T. ) ;
#17964 = ORIENTED_EDGE ( 'NONE', *, *, #4790, .T. ) ;
#17965 = ORIENTED_EDGE ( 'NONE', *, *, #22284, .F. ) ;
#17966 = DIRECTION ( 'NONE',  ( 0.000000000000000000, -1.000000000000000000, 0.000000000000000000 ) ) ;
#17967 = VERTEX_POINT ( 'NONE', #14049 ) ;
#17968 = ORIENTED_EDGE ( 'NONE', *, *, #15592, .F. ) ;
#17969 = APPROVAL_PERSON_ORGANIZATION ( #5897, #11912, #377 ) ;
#17970 = CARTESIAN_POINT ( 'NONE',  ( 6.222999999999998977, -3579.494999999999891, 2239.009999999999764 ) ) ;
#17971 = EDGE_CURVE ( 'NONE', #20881, #16359, #8006, .T. ) ;
#17972 = DATE_AND_TIME ( #19740, #13512 ) ;
#17973 = FACE_OUTER_BOUND ( 'NONE', #17540, .T. ) ;
#17974 = DIRECTION ( 'NONE',  ( 0.000000000000000000, 0.000000000000000000, -1.000000000000000000 ) ) ;
#17975 = ORIENTED_EDGE ( 'NONE', *, *, #12974, .T. ) ;
#17976 = DIRECTION ( 'NONE',  ( 0.000000000000000000, 0.8660254037838039931, 0.5000000000010993428 ) ) ;
#17977 = CARTESIAN_POINT ( 'NONE',  ( 9.855200508393231473, -3579.494999998446929, 2257.962940200991852 ) ) ;
#17978 = DIRECTION ( 'NONE',  ( -1.000000000000000000, 5.461016542361937364E-28, 2.336881798970999789E-14 ) ) ;
#17979 = DATE_AND_TIME ( #3684, #7519 ) ;
#17980 = ORIENTED_EDGE ( 'NONE', *, *, #3784, .F. ) ;
#17981 = CARTESIAN_POINT ( 'NONE',  ( 131.9776566397356703, -3543.802992058954260, 2260.344391216158328 ) ) ;
#17982 = VERTEX_POINT ( 'NONE', #12170 ) ;
#17983 = EDGE_CURVE ( 'NONE', #12671, #20881, #12290, .T. ) ;
#17984 = CIRCLE ( 'NONE', #3754, 0.7619999999999987894 ) ;
#17985 = EDGE_CURVE ( 'NONE', #21023, #6431, #14712, .T. ) ;
#17986 = CARTESIAN_POINT ( 'NONE',  ( -5.588000000000000078, -3660.140000000000327, 2247.392000000000280 ) ) ;
#17987 = DIRECTION ( 'NONE',  ( -1.000000000000000000, -0.000000000000000000, -0.000000000000000000 ) ) ;
#17988 = APPLIED_SECURITY_CLASSIFICATION_ASSIGNMENT ( #11243, ( #23165 ) ) ;
#17989 = APPROVAL_PERSON_ORGANIZATION ( #20040, #18779, #7384 ) ;
#17990 = ORIENTED_EDGE ( 'NONE', *, *, #1197, .F. ) ;
#17991 = DIRECTION ( 'NONE',  ( 0.000000000000000000, 0.000000000000000000, 1.000000000000000000 ) ) ;
#17992 = LINE ( 'NONE', #12721, #16638 ) ;
#17993 = CARTESIAN_POINT ( 'NONE',  ( 144.6787468485286752, -3576.681201580200195, 2245.535362107170840 ) ) ;
#17994 = DIRECTION ( 'NONE',  ( 1.000000000000000000, 0.000000000000000000, 0.000000000000000000 ) ) ;
#17995 = CARTESIAN_POINT ( 'NONE',  ( 10.36831320284000135, -3595.458900000000085, 2292.781800000000203 ) ) ;
#17996 = VERTEX_POINT ( 'NONE', #3260 ) ;
#17997 = AXIS2_PLACEMENT_3D ( 'NONE', #11637, #4397, #2523 ) ;
#17998 = CARTESIAN_POINT ( 'NONE',  ( 15.03168679717000167, -3660.851200000000063, 2242.820000000000164 ) ) ;
#17999 = ORIENTED_EDGE ( 'NONE', *, *, #11984, .T. ) ;
#18000 = PLANE ( 'NONE',  #19877 ) ;
#18001 = CARTESIAN_POINT ( 'NONE',  ( 76.20000000000000284, -3568.700000000000273, 2259.837999999999738 ) ) ;
#18002 = CARTESIAN_POINT ( 'NONE',  ( 139.6999999999999886, -3579.494999999999891, 2272.030000000000200 ) ) ;
#18003 = APPLICATION_CONTEXT ( 'configuration controlled 3d designs of mechanical parts and assemblies' ) ;
#18004 = FACE_OUTER_BOUND ( 'NONE', #2281, .T. ) ;
#18005 = CARTESIAN_POINT ( 'NONE',  ( 142.5377471795426345, -3543.413280444186512, 2255.028339697483716 ) ) ;
#18006 = CARTESIAN_POINT ( 'NONE',  ( 139.7000000001000046, -3656.812599999999748, 2242.820000000000164 ) ) ;
#18007 = APPLIED_APPROVAL_ASSIGNMENT ( #18213, ( #10136 ) ) ;
#18008 = EDGE_LOOP ( 'NONE', ( #17275, #11767, #7331, #6244 ) ) ;
#18009 = APPLIED_SECURITY_CLASSIFICATION_ASSIGNMENT ( #22059, ( #16085 ) ) ;
#18010 = CARTESIAN_POINT ( 'NONE',  ( 7.808657878250968132, -3576.539255533550659, 2245.746599050030454 ) ) ;
#18011 = ORIENTED_EDGE ( 'NONE', *, *, #13275, .T. ) ;
#18012 = CARTESIAN_POINT ( 'NONE',  ( -12.54218463272304085, -3661.486200000483223, 2249.723686796998663 ) ) ;
#18013 = CARTESIAN_POINT ( 'NONE',  ( 64.76999999999999602, -3568.700000000000273, 2286.368300000000090 ) ) ;
#18014 = AXIS2_PLACEMENT_3D ( 'NONE', #8389, #3571, #2047 ) ;
#18015 = CIRCLE ( 'NONE', #21398, 0.7619999999999294005 ) ;
#18016 = DIRECTION ( 'NONE',  ( -1.000000000000000000, 0.000000000000000000, 0.000000000000000000 ) ) ;
#18017 = CARTESIAN_POINT ( 'NONE',  ( 18.41499999999999915, -3639.502500000000055, 2295.829799999999977 ) ) ;
#18018 = DIRECTION ( 'NONE',  ( -1.000000000000000000, 0.000000000000000000, -1.344534956949000041E-13 ) ) ;
#18019 = CARTESIAN_POINT ( 'NONE',  ( 17.78000000000000114, -3639.502500000000055, 2296.210799999999836 ) ) ;
#18020 = EDGE_CURVE ( 'NONE', #15463, #7476, #6138, .T. ) ;
#18021 = EDGE_CURVE ( 'NONE', #17242, #22049, #20689, .T. ) ;
#18022 = EDGE_CURVE ( 'NONE', #18622, #4922, #17835, .T. ) ;
#18023 = CARTESIAN_POINT ( 'NONE',  ( 64.76999999999999602, -3670.300000000000182, 2286.368300000000090 ) ) ;
#18024 = ORIENTED_EDGE ( 'NONE', *, *, #20844, .F. ) ;
#18025 = CYLINDRICAL_SURFACE ( 'NONE', #595, 0.3809999999999121312 ) ;
#18026 = DIRECTION ( 'NONE',  ( -1.000000000000000000, 0.000000000000000000, 0.000000000000000000 ) ) ;
#18027 = VERTEX_POINT ( 'NONE', #17380 ) ;
#18028 = EDGE_CURVE ( 'NONE', #8967, #16380, #21841, .T. ) ;
#18029 = FACE_OUTER_BOUND ( 'NONE', #16330, .T. ) ;
#18030 = TOROIDAL_SURFACE ( 'NONE', #21415, 3.606799999998999695, 0.7620000000000000107 ) ;
#18031 = CIRCLE ( 'NONE', #17652, 2.844800000000001550 ) ;
#18032 = ORIENTED_EDGE ( 'NONE', *, *, #19335, .F. ) ;
#18033 = DIRECTION ( 'NONE',  ( 0.000000000000000000, 0.000000000000000000, 1.000000000000000000 ) ) ;
#18034 = CARTESIAN_POINT ( 'NONE',  ( 139.6999999999999886, -3582.187399999999798, 2242.820000000000164 ) ) ;
#18035 = ADVANCED_FACE ( 'NONE', ( #992 ), #22663, .T. ) ;
#18036 = EDGE_LOOP ( 'NONE', ( #9835, #9732, #6248, #18058 ) ) ;
#18037 = ADVANCED_FACE ( 'NONE', ( #1340 ), #8504, .T. ) ;
#18038 = CARTESIAN_POINT ( 'NONE',  ( 137.3036342121837379, -3581.028288794486343, 2249.234011237613686 ) ) ;
#18039 = ORIENTED_EDGE ( 'NONE', *, *, #15512, .T. ) ;
#18040 = SPHERICAL_SURFACE ( 'NONE', #7772, 0.7620000000000000107 ) ;
#18041 = CALENDAR_DATE ( 2026, 26, 10 ) ;
#18042 = DIRECTION ( 'NONE',  ( 1.000000000000000000, 0.000000000000000000, 0.000000000000000000 ) ) ;
#18043 = CARTESIAN_POINT ( 'NONE',  ( 11.34365660145000021, -3657.155744320999929, 2239.391000000000076 ) ) ;
#18044 = CIRCLE ( 'NONE', #19551, 5.080000000000000959 ) ;
#18045 = VECTOR ( 'NONE', #1606, 1000.000000000000000 ) ;
#18046 = CARTESIAN_POINT ( 'NONE',  ( 15.41268679728753099, -3577.928829547073747, 2239.009999999999764 ) ) ;
#18047 = DIRECTION ( 'NONE',  ( -0.8660254037820787065, -0.5000000000040877302, 0.000000000000000000 ) ) ;
#18048 = TOROIDAL_SURFACE ( 'NONE', #10554, 5.080000000000000071, 0.3810000000000000053 ) ;
#18049 = CARTESIAN_POINT ( 'NONE',  ( 138.4607614358540388, -3576.933900292242924, 2249.485745238374875 ) ) ;
#18050 = ORIENTED_EDGE ( 'NONE', *, *, #1277, .T. ) ;
#18051 = CARTESIAN_POINT ( 'NONE',  ( 134.5203320287740496, -3577.080245332521827, 2245.172503490672170 ) ) ;
#18052 = DIRECTION ( 'NONE',  ( 0.000000000000000000, 0.000000000000000000, -1.000000000000000000 ) ) ;
#18053 = ORIENTED_EDGE ( 'NONE', *, *, #13811, .F. ) ;
#18054 = DIRECTION ( 'NONE',  ( 0.000000000000000000, 0.000000000000000000, 1.000000000000000000 ) ) ;
#18055 = CARTESIAN_POINT ( 'NONE',  ( 0.000000000000000000, -3694.430000000000291, 2259.329999999999927 ) ) ;
#18056 = SHAPE_REPRESENTATION ( 'Screw 3', ( #5611 ), #16462 ) ;
#18057 = CIRCLE ( 'NONE', #1576, 2.844799999999994444 ) ;
#18058 = ORIENTED_EDGE ( 'NONE', *, *, #12964, .T. ) ;
#18059 = CARTESIAN_POINT ( 'NONE',  ( 15.33658054938999982, -3660.585448001000259, 2257.909769185999721 ) ) ;
#18060 = CARTESIAN_POINT ( 'NONE',  ( -6.730999999999999872, -3578.860000000000127, 2247.392000000000280 ) ) ;
#18061 = AXIS2_PLACEMENT_3D ( 'NONE', #13649, #13418, #22311 ) ;
#18062 = ORIENTED_EDGE ( 'NONE', *, *, #5347, .T. ) ;
#18063 = CIRCLE ( 'NONE', #7964, 0.7619999999999987894 ) ;
#18064 = DIRECTION ( 'NONE',  ( -1.000000000000000000, 0.000000000000000000, 0.000000000000000000 ) ) ;
#18065 = CARTESIAN_POINT ( 'NONE',  ( 9.855201422231997910, -3639.502499925999928, 2279.447341858000073 ) ) ;
#18066 =( LENGTH_UNIT ( ) NAMED_UNIT ( * ) SI_UNIT ( .MILLI., .METRE. ) );
#18067 = CARTESIAN_POINT ( 'NONE',  ( 9.652920519510999497, -3543.299999999999727, 2254.503999999999905 ) ) ;
#18068 = FACE_OUTER_BOUND ( 'NONE', #17946, .T. ) ;
#18069 = CALENDAR_DATE ( 2026, 26, 10 ) ;
#18070 = CARTESIAN_POINT ( 'NONE',  ( 3.048000000000000043, -3543.299999999999727, 2229.612000000000080 ) ) ;
#18071 = CARTESIAN_POINT ( 'NONE',  ( 9.802881971985723197, -3695.643849726979624, 2254.879006055995887 ) ) ;
#18072 = ORIENTED_EDGE ( 'NONE', *, *, #8810, .F. ) ;
#18073 = DIRECTION ( 'NONE',  ( 0.000000000000000000, 1.000000000000000000, 0.000000000000000000 ) ) ;
#18074 = AXIS2_PLACEMENT_3D ( 'NONE', #13167, #21958, #2727 ) ;
#18075 = CARTESIAN_POINT ( 'NONE',  ( 137.8181448509824918, -3657.371504566497606, 2248.046850338492732 ) ) ;
#18076 = ORIENTED_EDGE ( 'NONE', *, *, #10302, .F. ) ;
#18077 = ORIENTED_EDGE ( 'NONE', *, *, #2430, .F. ) ;
#18078 = AXIS2_PLACEMENT_3D ( 'NONE', #4478, #15272, #4259 ) ;
#18079 = CARTESIAN_POINT ( 'NONE',  ( 141.4070264929715393, -3661.780831764733193, 2249.715973214696533 ) ) ;
#18080 = APPLIED_PERSON_AND_ORGANIZATION_ASSIGNMENT ( #13006, #21788, ( #28 ) ) ;
#18081 = VERTEX_POINT ( 'NONE', #7177 ) ;
#18082 = ORIENTED_EDGE ( 'NONE', *, *, #13288, .F. ) ;
#18083 = DIRECTION ( 'NONE',  ( 0.000000000000000000, -1.000000000000000000, 0.000000000000000000 ) ) ;
#18084 = EDGE_CURVE ( 'NONE', #12318, #2684, #13607, .T. ) ;
#18085 = ORIENTED_EDGE ( 'NONE', *, *, #16429, .F. ) ;
#18086 = ORIENTED_EDGE ( 'NONE', *, *, #14939, .T. ) ;
#18087 = FACE_OUTER_BOUND ( 'NONE', #20074, .T. ) ;
#18088 = CARTESIAN_POINT ( 'NONE',  ( -12.54218463272850137, -3658.793799999516068, 2245.060313203004171 ) ) ;
#18089 = TOROIDAL_SURFACE ( 'NONE', #14353, 3.606799999999999784, 0.7620000000000000107 ) ;
#18090 = EDGE_CURVE ( 'NONE', #10469, #17185, #9131, .T. ) ;
#18091 = ORIENTED_EDGE ( 'NONE', *, *, #15138, .T. ) ;
#18092 = CARTESIAN_POINT ( 'NONE',  ( 142.0316867971999955, -3580.841199999999844, 2239.391000000000076 ) ) ;
#18093 = LINE ( 'NONE', #19394, #7855 ) ;
#18094 = CARTESIAN_POINT ( 'NONE',  ( -6.349999999999999645, -3544.061999999999898, 2253.487999999999829 ) ) ;
#18095 = VECTOR ( 'NONE', #13948, 1000.000000000000114 ) ;
#18096 = DIRECTION ( 'NONE',  ( 0.000000000000000000, 0.000000000000000000, 1.000000000000000000 ) ) ;
#18097 = APPROVAL_DATE_TIME ( #9198, #14387 ) ;
#18098 = CLOSED_SHELL ( 'NONE', ( #12828, #11542, #15237, #14531, #20699, #13376, #1126, #6408, #1718, #1204, #4670, #5843, #15150, #13009, #19400, #5545, #15106, #17752, #17956, #16392, #15766, #1831, #10107, #18971, #1799, #11649 ) ) ;
#18099 = CARTESIAN_POINT ( 'NONE',  ( 131.7715554716681936, -3543.401400258583635, 2259.827586953830632 ) ) ;
#18100 = ORIENTED_EDGE ( 'NONE', *, *, #1892, .F. ) ;
#18101 = CARTESIAN_POINT ( 'NONE',  ( 12.69999999999999929, -3599.497499999999945, 2296.210799999999836 ) ) ;
#18102 = CARTESIAN_POINT ( 'NONE',  ( 7.545491619780686499, -3661.969978295142482, 2245.207967436793297 ) ) ;
#18103 = EDGE_LOOP ( 'NONE', ( #22390, #22952, #15002, #5559 ) ) ;
#18104 = AXIS2_PLACEMENT_3D ( 'NONE', #3289, #8798, #21229 ) ;
#18105 = DIRECTION ( 'NONE',  ( -0.6887494619146010688, 0.000000000000000000, -0.7249994335945012525 ) ) ;
#18106 = DIRECTION ( 'NONE',  ( 0.000000000000000000, 0.000000000000000000, -1.000000000000000000 ) ) ;
#18107 = DIRECTION ( 'NONE',  ( -1.000000000000000000, -0.000000000000000000, -0.000000000000000000 ) ) ;
#18108 = CARTESIAN_POINT ( 'NONE',  ( 137.3683132029000262, -3658.158799999999701, 2242.820000000000164 ) ) ;
#18109 = FACE_OUTER_BOUND ( 'NONE', #684, .T. ) ;
#18110 = EDGE_CURVE ( 'NONE', #11279, #22077, #15413, .T. ) ;
#18111 = VERTEX_POINT ( 'NONE', #22775 ) ;
#18112 = CARTESIAN_POINT ( 'NONE',  ( 9.987313202947220248, -3601.063670452640054, 2296.591799999999694 ) ) ;
#18113 = EDGE_CURVE ( 'NONE', #15765, #10888, #19044, .T. ) ;
#18114 = DIRECTION ( 'NONE',  ( 0.000000000000000000, 0.000000000000000000, -1.000000000000000000 ) ) ;
#18115 = EDGE_CURVE ( 'NONE', #17042, #5087, #15297, .T. ) ;
#18116 = CARTESIAN_POINT ( 'NONE',  ( 88.90000000000000568, -3594.099999999999909, 2259.837999999999738 ) ) ;
#18117 = EDGE_CURVE ( 'NONE', #1860, #7174, #10998, .T. ) ;
#18118 = DIRECTION ( 'NONE',  ( -1.000000000000000000, 0.000000000000000000, 0.000000000000000000 ) ) ;
#18119 = CARTESIAN_POINT ( 'NONE',  ( 142.2400000000000091, -3544.570000000000164, 2255.774000000000342 ) ) ;
#18120 = DIRECTION ( 'NONE',  ( -5.666055098014000101E-14, 3.885294924352999876E-13, -1.000000000000000000 ) ) ;
#18121 = AXIS2_PLACEMENT_3D ( 'NONE', #17667, #5026, #23055 ) ;
#18122 = CARTESIAN_POINT ( 'NONE',  ( 7.457719349988209068, -3577.219030987115730, 2245.067999188746398 ) ) ;
#18123 = ORIENTED_EDGE ( 'NONE', *, *, #9373, .T. ) ;
#18124 = SHAPE_DEFINITION_REPRESENTATION ( #237, #20448 ) ;
#18125 = TOROIDAL_SURFACE ( 'NONE', #21128, 1.905000000000000027, 1.270000000000000018 ) ;
#18126 = DIRECTION ( 'NONE',  ( 0.000000000000000000, 0.000000000000000000, -1.000000000000000000 ) ) ;
#18127 = CARTESIAN_POINT ( 'NONE',  ( 55.57575231171000496, -3695.699999999999818, 2275.763800000000174 ) ) ;
#18128 = APPROVAL_DATE_TIME ( #10982, #18213 ) ;
#18129 = DIRECTION ( 'NONE',  ( 0.000000000000000000, 0.000000000000000000, -1.000000000000000000 ) ) ;
#18130 = DIRECTION ( 'NONE',  ( 0.000000000000000000, 1.000000000000000000, 0.000000000000000000 ) ) ;
#18131 = EDGE_LOOP ( 'NONE', ( #10330, #17282, #22273, #11088 ) ) ;
#18132 = DIRECTION ( 'NONE',  ( 2.336881798971000105E-14, 2.336881798971000105E-14, 1.000000000000000000 ) ) ;
#18133 = ORIENTED_EDGE ( 'NONE', *, *, #16140, .T. ) ;
#18134 = AXIS2_PLACEMENT_3D ( 'NONE', #1355, #5120, #8520 ) ;
#18135 = CYLINDRICAL_SURFACE ( 'NONE', #15568, 2.844799999999999773 ) ;
#18136 = VECTOR ( 'NONE', #7452, 1000.000000000000000 ) ;
#18137 = CARTESIAN_POINT ( 'NONE',  ( 12.07304487791000192, -3636.721615716000088, 2279.801384127999881 ) ) ;
#18138 = VECTOR ( 'NONE', #14001, 1000.000000000000000 ) ;
#18139 = EDGE_LOOP ( 'NONE', ( #10965, #2555, #8723, #20755 ) ) ;
#18140 = LINE ( 'NONE', #5964, #2436 ) ;
#18141 = ADVANCED_FACE ( 'NONE', ( #2873 ), #15525, .F. ) ;
#18142 = VERTEX_POINT ( 'NONE', #6932 ) ;
#18143 = CARTESIAN_POINT ( 'NONE',  ( 142.2400000000000091, -3694.430000000000291, 2255.774000000000342 ) ) ;
#18144 = CARTESIAN_POINT ( 'NONE',  ( 50.79999999999999716, -3568.700000000000273, 2239.771999999999935 ) ) ;
#18145 = VERTEX_POINT ( 'NONE', #12 ) ;
#18146 = EDGE_CURVE ( 'NONE', #15124, #1232, #512, .T. ) ;
#18147 = EDGE_CURVE ( 'NONE', #8337, #13988, #1620, .T. ) ;
#18148 = CARTESIAN_POINT ( 'NONE',  ( 137.5529558738440983, -3581.361364689894344, 2248.747063143178821 ) ) ;
#18149 = ORIENTED_EDGE ( 'NONE', *, *, #13090, .T. ) ;
#18150 = DIRECTION ( 'NONE',  ( 0.000000000000000000, 1.000000000000000000, 0.000000000000000000 ) ) ;
#18151 = TOROIDAL_SURFACE ( 'NONE', #15902, 3.606799999998999695, 0.7620000000000000107 ) ;
#18152 = DATE_TIME_ROLE ( 'classification_date' ) ;
#18153 = VECTOR ( 'NONE', #6106, 1000.000000000000000 ) ;
#18154 = DIRECTION ( 'NONE',  ( -1.000000000000000000, 0.000000000000000000, 0.000000000000000000 ) ) ;
#18155 = DIRECTION ( 'NONE',  ( 1.000000000000000000, 0.000000000000000000, 0.000000000000000000 ) ) ;
#18156 = EDGE_CURVE ( 'NONE', #2684, #20725, #16059, .T. ) ;
#18157 = DIRECTION ( 'NONE',  ( 0.000000000000000000, 1.000000000000000000, 0.000000000000000000 ) ) ;
#18158 = CARTESIAN_POINT ( 'NONE',  ( 10.21049783562821034, -3640.939814744883734, 2296.591799999930572 ) ) ;
#18159 = CARTESIAN_POINT ( 'NONE',  ( 141.7805098429321333, -3577.552631540255788, 2249.919755263941170 ) ) ;
#18160 = ORIENTED_EDGE ( 'NONE', *, *, #21305, .T. ) ;
#18161 = CARTESIAN_POINT ( 'NONE',  ( 134.6795851643913693, -3576.764266229913119, 2245.468189507787883 ) ) ;
#18162 = EDGE_CURVE ( 'NONE', #3671, #16761, #2733, .T. ) ;
#18163 = EDGE_CURVE ( 'NONE', #11209, #3129, #7612, .T. ) ;
#18164 = CARTESIAN_POINT ( 'NONE',  ( 133.2229999999999848, -3659.504999999999654, 2239.009999999999764 ) ) ;
#18165 = VERTEX_POINT ( 'NONE', #6703 ) ;
#18166 = VECTOR ( 'NONE', #4166, 1000.000000000000114 ) ;
#18167 = CARTESIAN_POINT ( 'NONE',  ( 14.21033367406000103, -3597.079566860000341, 2279.715678855999613 ) ) ;
#18168 = FACE_OUTER_BOUND ( 'NONE', #16732, .T. ) ;
#18169 = AXIS2_PLACEMENT_3D ( 'NONE', #12296, #14178, #17438 ) ;
#18170 = APPLICATION_CONTEXT ( 'configuration controlled 3d designs of mechanical parts and assemblies' ) ;
#18171 = VECTOR ( 'NONE', #9466, 1000.000000000000114 ) ;
#18172 = VERTEX_POINT ( 'NONE', #13843 ) ;
#18173 = DIRECTION ( 'NONE',  ( 7.280632624815999719E-13, -1.000000000000000000, 4.288485907148999414E-12 ) ) ;
#18174 = DIRECTION ( 'NONE',  ( -1.073225997510925892E-13, 0.000000000000000000, -1.000000000000000000 ) ) ;
#18175 = AXIS2_PLACEMENT_3D ( 'NONE', #7500, #9792, #14658 ) ;
#18176 = ORIENTED_EDGE ( 'NONE', *, *, #21864, .F. ) ;
#18177 = CYLINDRICAL_SURFACE ( 'NONE', #7766, 1.269999999999882334 ) ;
#18178 = EDGE_CURVE ( 'NONE', #12834, #6172, #17815, .T. ) ;
#18179 = DIRECTION ( 'NONE',  ( 1.000000000000000000, 0.000000000000000000, 0.000000000000000000 ) ) ;
#18180 = AXIS2_PLACEMENT_3D ( 'NONE', #8239, #6489, #21015 ) ;
#18181 = CARTESIAN_POINT ( 'NONE',  ( 141.5378770596536526, -3581.666564005086911, 2246.925237844513958 ) ) ;
#18182 = EDGE_LOOP ( 'NONE', ( #10184, #10043, #18366, #14862 ) ) ;
#18183 = CARTESIAN_POINT ( 'NONE',  ( 15.03168679714000078, -3640.848700000000008, 2292.781800000000203 ) ) ;
#18184 = APPROVAL_STATUS ( 'not_yet_approved' ) ;
#18185 = DIRECTION ( 'NONE',  ( 0.000000000000000000, 0.000000000000000000, 1.000000000000000000 ) ) ;
#18186 = CYLINDRICAL_SURFACE ( 'NONE', #10932, 2.844800000000091700 ) ;
#18187 = ORIENTED_EDGE ( 'NONE', *, *, #7962, .T. ) ;
#18188 = DIRECTION ( 'NONE',  ( -0.8660254037821217832, -0.5000000000040129011, 0.000000000000000000 ) ) ;
#18189 = VECTOR ( 'NONE', #5711, 1000.000000000000114 ) ;
#18190 = AXIS2_PLACEMENT_3D ( 'NONE', #8282, #13673, #777 ) ;
#18191 = CARTESIAN_POINT ( 'NONE',  ( 137.5756652831487656, -3657.612887080431847, 2248.698366170355257 ) ) ;
#18192 = AXIS2_PLACEMENT_3D ( 'NONE', #7132, #14280, #17780 ) ;
#18193 = EDGE_LOOP ( 'NONE', ( #617, #7399 ) ) ;
#18194 = CARTESIAN_POINT ( 'NONE',  ( 141.0596176031389746, -3662.005499788756879, 2249.540428743966004 ) ) ;
#18195 = EDGE_CURVE ( 'NONE', #10683, #7794, #5013, .T. ) ;
#18196 = CIRCLE ( 'NONE', #5483, 0.7619999999999294005 ) ;
#18197 = AXIS2_PLACEMENT_3D ( 'NONE', #3345, #14023, #8628 ) ;
#18198 = ORIENTED_EDGE ( 'NONE', *, *, #18311, .T. ) ;
#18199 = VERTEX_POINT ( 'NONE', #12196 ) ;
#18200 = FACE_OUTER_BOUND ( 'NONE', #1935, .T. ) ;
#18201 = ORIENTED_EDGE ( 'NONE', *, *, #9010, .F. ) ;
#18202 = ORIENTED_EDGE ( 'NONE', *, *, #14715, .F. ) ;
#18203 = DIRECTION ( 'NONE',  ( -0.000000000000000000, 1.000000000000000000, 0.000000000000000000 ) ) ;
#18204 = LINE ( 'NONE', #14470, #2438 ) ;
#18205 = VERTEX_POINT ( 'NONE', #14197 ) ;
#18206 = TOROIDAL_SURFACE ( 'NONE', #1737, 1.905000000000000027, 1.270000000000000018 ) ;
#18207 = CARTESIAN_POINT ( 'NONE',  ( 137.3683132029000262, -3658.158799999999701, 2242.820000000000164 ) ) ;
#18208 = FACE_OUTER_BOUND ( 'NONE', #6946, .T. ) ;
#18209 = CARTESIAN_POINT ( 'NONE',  ( 1.270000000000000018, -3694.430000000000291, 2259.329999999999927 ) ) ;
#18210 = DIRECTION ( 'NONE',  ( 2.324635735433000053E-14, 0.000000000000000000, 1.000000000000000000 ) ) ;
#18211 = VECTOR ( 'NONE', #22990, 1000.000000000000000 ) ;
#18212 = DATE_TIME_ROLE ( 'creation_date' ) ;
#18213 = APPROVAL ( #16257, 'UNKNOWN' ) ;
#18214 = CARTESIAN_POINT ( 'NONE',  ( 139.6999999999999886, -3659.504999999999654, 2245.359999999999673 ) ) ;
#18215 = EDGE_LOOP ( 'NONE', ( #17787, #1753, #13358, #13528 ) ) ;
#18216 = DIRECTION ( 'NONE',  ( -1.000000000000000000, 0.000000000000000000, 0.000000000000000000 ) ) ;
#18217 = DIRECTION ( 'NONE',  ( -1.224646799147353207E-16, 1.000000000000000000, 0.000000000000000000 ) ) ;
#18218 = CARTESIAN_POINT ( 'NONE',  ( 12.69999999999999929, -3579.494999999999891, 2255.774000000000342 ) ) ;
#18219 = ORIENTED_EDGE ( 'NONE', *, *, #6233, .T. ) ;
#18220 = AXIS2_PLACEMENT_3D ( 'NONE', #23103, #21017, #19256 ) ;
#18221 = DIRECTION ( 'NONE',  ( 0.000000000000000000, 0.000000000000000000, -1.000000000000000000 ) ) ;
#18222 = AXIS2_PLACEMENT_3D ( 'NONE', #19749, #7325, #14478 ) ;
#18223 = DIRECTION ( 'NONE',  ( -0.5000000000040877302, 0.8660254037820785955, 0.000000000000000000 ) ) ;
#18224 = CARTESIAN_POINT ( 'NONE',  ( -6.731000000000127770, -3578.860000000000127, 2241.931000000000040 ) ) ;
#18225 = CARTESIAN_POINT ( 'NONE',  ( 15.87499999990501287, -3694.938000000000102, 2281.351800000094954 ) ) ;
#18226 = DIRECTION ( 'NONE',  ( 0.000000000000000000, 1.000000000000000000, 0.000000000000000000 ) ) ;
#18227 = CIRCLE ( 'NONE', #2903, 3.175000000000149925 ) ;
#18228 = ORIENTED_EDGE ( 'NONE', *, *, #1417, .F. ) ;
#18229 = DIRECTION ( 'NONE',  ( 0.000000000000000000, 0.000000000000000000, 1.000000000000000000 ) ) ;
#18230 = CARTESIAN_POINT ( 'NONE',  ( 12.69999999999999929, -3639.502500000000055, 2263.571799999999712 ) ) ;
#18231 = CARTESIAN_POINT ( 'NONE',  ( 57.14999999999999858, -3544.570000000000164, 2250.236800000000130 ) ) ;
#18232 = CARTESIAN_POINT ( 'NONE',  ( 12.69999999999999929, -3639.502500000000055, 2281.351799999999912 ) ) ;
#18233 = CARTESIAN_POINT ( 'NONE',  ( 142.1895021645321151, -3578.057685255049364, 2239.009999999921547 ) ) ;
#18234 = FACE_OUTER_BOUND ( 'NONE', #21829, .T. ) ;
#18235 = ORIENTED_EDGE ( 'NONE', *, *, #15896, .F. ) ;
#18236 = PERSON_AND_ORGANIZATION ( #5446, #1895 ) ;
#18237 = APPROVAL ( #22779, 'UNSPECIFIED' ) ;
#18238 = VECTOR ( 'NONE', #18296, 1000.000000000000000 ) ;
#18239 = CARTESIAN_POINT ( 'NONE',  ( -12.54218463257254612, -3657.447599999590238, 2247.391999999993914 ) ) ;
#18240 = DIRECTION ( 'NONE',  ( -3.591349225554024811E-12, 0.5000000000004030110, -0.8660254037842058938 ) ) ;
#18241 = PERSON_AND_ORGANIZATION_ROLE ( 'classification_officer' ) ;
#18242 = AXIS2_PLACEMENT_3D ( 'NONE', #12401, #8890, #10873 ) ;
#18243 = DIRECTION ( 'NONE',  ( 1.000000000000000000, -2.848812946084999742E-12, 0.000000000000000000 ) ) ;
#18244 = EDGE_CURVE ( 'NONE', #1840, #12928, #16598, .T. ) ;
#18245 = DIRECTION ( 'NONE',  ( -1.000000000000000000, 0.000000000000000000, 0.000000000000000000 ) ) ;
#18246 = ADVANCED_FACE ( 'NONE', ( #4930 ), #3887, .T. ) ;
#18247 = DIRECTION ( 'NONE',  ( 0.5000000000040877302, 0.8660254037820785955, 0.000000000000000000 ) ) ;
#18248 = EDGE_CURVE ( 'NONE', #19266, #22749, #13994, .T. ) ;
#18249 = ORIENTED_EDGE ( 'NONE', *, *, #5818, .T. ) ;
#18250 = DIRECTION ( 'NONE',  ( 1.730170395987526852E-13, -1.000000000000000000, 0.000000000000000000 ) ) ;
#18251 = ORIENTED_EDGE ( 'NONE', *, *, #11983, .T. ) ;
#18252 = FACE_OUTER_BOUND ( 'NONE', #12648, .T. ) ;
#18253 = VECTOR ( 'NONE', #7126, 999.9999999999998863 ) ;
#18254 = CARTESIAN_POINT ( 'NONE',  ( 101.5999999999999943, -3619.500000000000000, 2261.869999999999891 ) ) ;
#18255 = ORIENTED_EDGE ( 'NONE', *, *, #15005, .T. ) ;
#18256 = ADVANCED_FACE ( 'NONE', ( #12427 ), #10611, .T. ) ;
#18257 = FACE_OUTER_BOUND ( 'NONE', #18687, .T. ) ;
#18258 = CIRCLE ( 'NONE', #22001, 2.844800000000091700 ) ;
#18259 = VERTEX_POINT ( 'NONE', #19461 ) ;
#18260 = CARTESIAN_POINT ( 'NONE',  ( 142.5315320345694090, -3695.579670240429095, 2255.043779575609278 ) ) ;
#18261 = DIRECTION ( 'NONE',  ( -0.000000000000000000, 0.000000000000000000, 1.000000000000000000 ) ) ;
#18262 = EDGE_CURVE ( 'NONE', #6249, #4922, #12487, .T. ) ;
#18263 = VERTEX_POINT ( 'NONE', #1641 ) ;
#18264 = DIRECTION ( 'NONE',  ( -9.070589041464213634E-14, 0.000000000000000000, -1.000000000000000000 ) ) ;
#18265 = EDGE_LOOP ( 'NONE', ( #22207, #22368 ) ) ;
#18266 = CARTESIAN_POINT ( 'NONE',  ( 145.1763627461602653, -3581.130155333931725, 2245.675470994407078 ) ) ;
#18267 = PERSON_AND_ORGANIZATION_ROLE ( 'design_supplier' ) ;
#18268 = CIRCLE ( 'NONE', #8171, 0.7619999999999294005 ) ;
#18269 = CARTESIAN_POINT ( 'NONE',  ( 76.20000000000000284, -3568.700000000000273, 2239.771999999999935 ) ) ;
#18270 = DIRECTION ( 'NONE',  ( 0.000000000000000000, 0.000000000000000000, 1.000000000000000000 ) ) ;
#18271 = DIRECTION ( 'NONE',  ( 1.073225997510925892E-13, 0.000000000000000000, 1.000000000000000000 ) ) ;
#18272 = EDGE_CURVE ( 'NONE', #22006, #10186, #16956, .T. ) ;
#18273 = CARTESIAN_POINT ( 'NONE',  ( 9.987313202947046165, -3641.068670452640163, 2296.591799999999694 ) ) ;
#18274 = CARTESIAN_POINT ( 'NONE',  ( 142.3112457684844685, -3578.363551668762284, 2250.194032828429954 ) ) ;
#18275 = B_SPLINE_CURVE_WITH_KNOTS ( 'NONE', 3,
 ( #10111, #13633, #19028, #855, #11878, #8139, #2967, #20541, #17257, #7903, #6622, #20435, #15283, #13514, #9999, #18672, #13405, #8021, #6384, #18785, #20654, #15168, #13760, #4384, #20904, #4839, #11990, #19143, #6271, #3082, #4491 ),
 .UNSPECIFIED., .F., .F.,
 ( 4, 2, 2, 2, 2, 2, 1, 2, 2, 2, 2, 1, 1, 2, 2, 2, 4 ),
 ( 0.000000000000000000, 0.1249999999979858889, 0.1874999999967077724, 0.2499999999954296559, 0.3749999999932559502, 0.4374999999922616900, 0.4687499999917597027, 0.4843749999919371718, 0.4999999999921146410, 0.6249999999960471619, 0.6874999999979408694, 0.7187499999991345812, 0.7343749999999843459, 0.7421875000001566525, 0.7500000000003289591, 0.8750000000001644240, 1.000000000000000000 ),
 .UNSPECIFIED. ) ;
#18276 = ORIENTED_EDGE ( 'NONE', *, *, #8557, .F. ) ;
#18277 = CARTESIAN_POINT ( 'NONE',  ( 134.2879922902995418, -3577.658673733719752, 2244.812092252487219 ) ) ;
#18278 = EDGE_CURVE ( 'NONE', #11706, #14933, #2388, .T. ) ;
#18279 = EDGE_CURVE ( 'NONE', #10484, #21098, #17694, .T. ) ;
#18280 = EDGE_LOOP ( 'NONE', ( #7704, #8372, #17609, #3781 ) ) ;
#18281 = CARTESIAN_POINT ( 'NONE',  ( 101.5999999999999943, -3619.500000000000000, 2259.837999999999738 ) ) ;
#18282 = EDGE_LOOP ( 'NONE', ( #11648, #5540, #10166, #6969 ) ) ;
#18283 = AXIS2_PLACEMENT_3D ( 'NONE', #400, #5804, #2279 ) ;
#18284 = DIRECTION ( 'NONE',  ( 0.000000000000000000, 0.000000000000000000, -1.000000000000000000 ) ) ;
#18285 = CARTESIAN_POINT ( 'NONE',  ( 12.69999999999999929, -3664.965999999999894, 2244.978999999999814 ) ) ;
#18286 = VERTEX_POINT ( 'NONE', #5051 ) ;
#18287 = CARTESIAN_POINT ( 'NONE',  ( -8.890000000032001637, -3577.513800000000174, 2245.060313203000078 ) ) ;
#18288 = CARTESIAN_POINT ( 'NONE',  ( 64.76999999999999602, -3568.700000000000273, 2289.213099999999940 ) ) ;
#18289 = ADVANCED_FACE ( 'NONE', ( #10434 ), #12129, .T. ) ;
#18290 = AXIS2_PLACEMENT_3D ( 'NONE', #21500, #12416, #231 ) ;
#18291 = VERTEX_POINT ( 'NONE', #1526 ) ;
#18292 = CARTESIAN_POINT ( 'NONE',  ( 9.855199999999999960, -3599.497499999999945, 2263.571799999999712 ) ) ;
#18293 = CARTESIAN_POINT ( 'NONE',  ( 15.09345051701841456, -3577.955111082732856, 2250.090084402730099 ) ) ;
#18294 = PLANE ( 'NONE',  #7942 ) ;
#18295 = VERTEX_POINT ( 'NONE', #3866 ) ;
#18296 = DIRECTION ( 'NONE',  ( 0.000000000000000000, 1.000000000000000000, 0.000000000000000000 ) ) ;
#18297 = EDGE_CURVE ( 'NONE', #7984, #17318, #22346, .T. ) ;
#18298 = CALENDAR_DATE ( 2026, 26, 10 ) ;
#18299 = DIRECTION ( 'NONE',  ( 0.000000000000000000, 0.000000000000000000, -1.000000000000000000 ) ) ;
#18300 = CYLINDRICAL_SURFACE ( 'NONE', #9451, 2.844800000000091700 ) ;
#18301 = ORIENTED_EDGE ( 'NONE', *, *, #18278, .F. ) ;
#18302 = CARTESIAN_POINT ( 'NONE',  ( -12.54218463262903605, -3661.486200000482768, 2245.060313202995985 ) ) ;
#18303 = CARTESIAN_POINT ( 'NONE',  ( 136.8737869705807384, -3579.119982125134811, 2257.957971615415772 ) ) ;
#18304 = ORIENTED_EDGE ( 'NONE', *, *, #17890, .F. ) ;
#18305 = ORIENTED_EDGE ( 'NONE', *, *, #8808, .T. ) ;
#18306 = CIRCLE ( 'NONE', #8203, 0.7619999999999294005 ) ;
#18307 = CARTESIAN_POINT ( 'NONE',  ( 140.7875140777326237, -3662.134083993774311, 2249.421034100285851 ) ) ;
#18308 = ADVANCED_FACE ( 'NONE', ( #2673 ), #911, .T. ) ;
#18309 = ADVANCED_FACE ( 'NONE', ( #22586 ), #5028, .T. ) ;
#18310 = ORIENTED_EDGE ( 'NONE', *, *, #1401, .T. ) ;
#18311 = EDGE_CURVE ( 'NONE', #13681, #21672, #696, .T. ) ;
#18312 = ORIENTED_EDGE ( 'NONE', *, *, #19626, .T. ) ;
#18313 = DIRECTION ( 'NONE',  ( 0.000000000000000000, 0.8660254037817070039, -0.5000000000047313264 ) ) ;
#18314 = ORIENTED_EDGE ( 'NONE', *, *, #8648, .F. ) ;
#18315 = SPHERICAL_SURFACE ( 'NONE', #4177, 0.7620000000000000107 ) ;
#18316 = DIRECTION ( 'NONE',  ( -2.994914837526000224E-13, 2.590196616237999979E-13, -1.000000000000000000 ) ) ;
#18317 = ADVANCED_FACE ( 'NONE', ( #6210 ), #11691, .T. ) ;
#18318 = AXIS2_PLACEMENT_3D ( 'NONE', #8041, #20682, #18931 ) ;
#18319 = ORIENTED_EDGE ( 'NONE', *, *, #2424, .F. ) ;
#18320 = FACE_OUTER_BOUND ( 'NONE', #14081, .T. ) ;
#18321 = DIRECTION ( 'NONE',  ( -1.000000000000000000, -9.561467977825999598E-14, 0.000000000000000000 ) ) ;
#18322 = CIRCLE ( 'NONE', #10081, 6.349999999999855760 ) ;
#18323 = CARTESIAN_POINT ( 'NONE',  ( 152.4000000000000057, -3544.061999999999898, 2275.763800000000174 ) ) ;
#18324 = ADVANCED_FACE ( 'NONE', ( #18846 ), #15455, .T. ) ;
#18325 = SHAPE_DEFINITION_REPRESENTATION ( #3388, #18056 ) ;
#18326 = EDGE_CURVE ( 'NONE', #6441, #21367, #9145, .T. ) ;
#18327 = DIRECTION ( 'NONE',  ( 0.000000000000000000, 0.000000000000000000, -1.000000000000000000 ) ) ;
#18328 = EDGE_LOOP ( 'NONE', ( #8147, #555, #7752, #20615 ) ) ;
#18329 = DIRECTION ( 'NONE',  ( 0.000000000000000000, 0.000000000000000000, 1.000000000000000000 ) ) ;
#18330 = CARTESIAN_POINT ( 'NONE',  ( 7.860134522445388683, -3662.544182877184085, 2245.871063940706790 ) ) ;
#18331 = ORIENTED_EDGE ( 'NONE', *, *, #20802, .T. ) ;
#18332 = DIRECTION ( 'NONE',  ( -2.848935406719999894E-12, 1.000000000000000000, 0.000000000000000000 ) ) ;
#18333 = AXIS2_PLACEMENT_3D ( 'NONE', #14071, #8909, #1634 ) ;
#18334 = LOCAL_TIME ( 17, 37, 43.00000000000000000, #7296 ) ;
#18335 = DIRECTION ( 'NONE',  ( 1.224646799147353207E-16, 1.000000000000000000, -0.000000000000000000 ) ) ;
#18336 = AXIS2_PLACEMENT_3D ( 'NONE', #712, #4005, #11153 ) ;
#18337 = CARTESIAN_POINT ( 'NONE',  ( 59.89320000000000022, -3594.099999999999909, 2239.771999999999935 ) ) ;
#18338 = CARTESIAN_POINT ( 'NONE',  ( 141.4351164934280121, -3581.757009752985596, 2257.727830821389489 ) ) ;
#18339 = CARTESIAN_POINT ( 'NONE',  ( 147.7412001510571997, -3543.315277321059966, 2259.544298694426743 ) ) ;
#18340 = EDGE_LOOP ( 'NONE', ( #16715, #11172, #19527, #16891 ) ) ;
#18341 = DIRECTION ( 'NONE',  ( 0.000000000000000000, 0.000000000000000000, -1.000000000000000000 ) ) ;
#18342 = CARTESIAN_POINT ( 'NONE',  ( 142.2400000000000091, -3694.430000000000291, 2255.774000000000342 ) ) ;
#18343 = B_SPLINE_CURVE_WITH_KNOTS ( 'NONE', 3,
 ( #6891, #11797, #20700, #3243 ),
 .UNSPECIFIED., .F., .F.,
 ( 4, 4 ),
 ( 0.000000000000000000, 1.000000000000000000 ),
 .UNSPECIFIED. ) ;
#18344 = CARTESIAN_POINT ( 'NONE',  ( 9.525000000266215849, -3543.615630734461320, 2281.351799999999912 ) ) ;
#18345 = DIRECTION ( 'NONE',  ( -1.000000000000000000, -0.000000000000000000, -0.000000000000000000 ) ) ;
#18346 = DIRECTION ( 'NONE',  ( 1.000000000000000000, 5.432398939370943590E-28, -2.324635735433000369E-14 ) ) ;
#18347 = DIRECTION ( 'NONE',  ( 0.000000000000000000, 0.000000000000000000, 1.000000000000000000 ) ) ;
#18348 = ORIENTED_EDGE ( 'NONE', *, *, #8429, .T. ) ;
#18350 = AXIS2_PLACEMENT_3D ( 'NONE', #4179, #9236, #440 ) ;
#18349 = APPLICATION_PROTOCOL_DEFINITION ( 'international standard', 'automotive_design', 2000, #12012 ) ;
#18351 = ORIENTED_EDGE ( 'NONE', *, *, #8733, .T. ) ;
#18352 = CARTESIAN_POINT ( 'NONE',  ( 134.6199999999999761, -3579.494999999999891, 2239.391000000000076 ) ) ;
#18353 = APPLIED_SECURITY_CLASSIFICATION_ASSIGNMENT ( #5262, ( #741 ) ) ;
#18354 = PRODUCT_DEFINITION_FORMATION_WITH_SPECIFIED_SOURCE ( 'ANY', '', #10501, .NOT_KNOWN. ) ;
#18355 = CARTESIAN_POINT ( 'NONE',  ( 151.1299999999999955, -3543.299999999999727, 2240.279999999999745 ) ) ;
#18356 = DIRECTION ( 'NONE',  ( 0.000000000000000000, 0.000000000000000000, -1.000000000000000000 ) ) ;
#18357 = EDGE_LOOP ( 'NONE', ( #21495, #3337 ) ) ;
#18358 = CARTESIAN_POINT ( 'NONE',  ( 137.3683132029000262, -3660.851200000000063, 2242.820000000000164 ) ) ;
#18359 = ORIENTED_EDGE ( 'NONE', *, *, #1663, .F. ) ;
#18360 = DIRECTION ( 'NONE',  ( 0.000000000000000000, 0.000000000000000000, -1.000000000000000000 ) ) ;
#18361 = ORIENTED_EDGE ( 'NONE', *, *, #4837, .T. ) ;
#18362 = DIRECTION ( 'NONE',  ( 0.000000000000000000, 0.000000000000000000, -1.000000000000000000 ) ) ;
#18363 = APPLIED_PERSON_AND_ORGANIZATION_ASSIGNMENT ( #1897, #12565, ( #2608 ) ) ;
#18364 = EDGE_CURVE ( 'NONE', #13145, #19144, #7846, .T. ) ;
#18365 = FACE_OUTER_BOUND ( 'NONE', #13194, .T. ) ;
#18366 = ORIENTED_EDGE ( 'NONE', *, *, #3222, .T. ) ;
#18367 = LOCAL_TIME ( 17, 37, 43.00000000000000000, #16029 ) ;
#18368 = PLANE ( 'NONE',  #16641 ) ;
#18369 = LOCAL_TIME ( 17, 37, 43.00000000000000000, #11293 ) ;
#18370 = CYLINDRICAL_SURFACE ( 'NONE', #18549, 1.269999999999882334 ) ;
#18371 = ADVANCED_FACE ( 'NONE', ( #8308 ), #11817, .T. ) ;
#18372 = VERTEX_POINT ( 'NONE', #6440 ) ;
#18373 = CARTESIAN_POINT ( 'NONE',  ( 73.35520000000001062, -3568.700000000000273, 2239.771999999999935 ) ) ;
#18374 = DIRECTION ( 'NONE',  ( 0.000000000000000000, 0.000000000000000000, 1.000000000000000000 ) ) ;
#18375 = EDGE_CURVE ( 'NONE', #15488, #20927, #20721, .T. ) ;
#18376 = ORIENTED_EDGE ( 'NONE', *, *, #19383, .T. ) ;
#18377 = EDGE_CURVE ( 'NONE', #3900, #14108, #13226, .T. ) ;
#18378 = CIRCLE ( 'NONE', #17997, 0.3810000000000002829 ) ;
#18379 = DIRECTION ( 'NONE',  ( -0.8660254037817187722, 0.5000000000047108983, 0.000000000000000000 ) ) ;
#18380 = PRODUCT_DEFINITION_CONTEXT ( 'detailed design', #7232, 'design' ) ;
#18381 = EDGE_LOOP ( 'NONE', ( #13333, #2179, #21, #17733, #11003, #19413, #14965, #24 ) ) ;
#18382 = CYLINDRICAL_SURFACE ( 'NONE', #17121, 0.3810000000000151599 ) ;
#18383 = APPROVAL_STATUS ( 'not_yet_approved' ) ;
#18384 = LINE ( 'NONE', #13007, #8 ) ;
#18385 = EDGE_CURVE ( 'NONE', #13823, #15748, #2032, .T. ) ;
#18386 = ORGANIZATION ( 'NAUO-ORG15', 'UNSPECIFIED', 'UNSPECIFIED' ) ;
#18387 = CARTESIAN_POINT ( 'NONE',  ( 17.96576512614983301, -3661.726329895977869, 2245.029840763826087 ) ) ;
#18388 = PLANE ( 'NONE',  #3251 ) ;
#18389 = DIRECTION ( 'NONE',  ( -1.000000000000000000, 0.000000000000000000, 0.000000000000000000 ) ) ;
#18390 = CARTESIAN_POINT ( 'NONE',  ( 139.9692956761142000, -3576.650356814839597, 2249.183748893157372 ) ) ;
#18391 = EDGE_LOOP ( 'NONE', ( #20960, #4678, #16072, #6449 ) ) ;
#18392 = AXIS2_PLACEMENT_3D ( 'NONE', #13783, #17278, #4863 ) ;
#18393 = AXIS2_PLACEMENT_3D ( 'NONE', #5911, #11282, #4137 ) ;
#18394 = CARTESIAN_POINT ( 'NONE',  ( 116.8400000000000034, -3695.699999999999818, 2247.392000000000280 ) ) ;
#18395 = EDGE_LOOP ( 'NONE', ( #21437, #2208 ) ) ;
#18396 = CARTESIAN_POINT ( 'NONE',  ( 13.01510790209939827, -3596.664354860411095, 2279.814648369741462 ) ) ;
#18397 = CARTESIAN_POINT ( 'NONE',  ( 15.38817332932362802, -3543.672816122930726, 2255.402926848485095 ) ) ;
#18398 = EDGE_CURVE ( 'NONE', #2146, #20703, #3512, .T. ) ;
#18399 = ORIENTED_EDGE ( 'NONE', *, *, #22579, .F. ) ;
#18400 = CARTESIAN_POINT ( 'NONE',  ( 12.69999999999999929, -3599.497499999999945, 2263.571799999999712 ) ) ;
#18401 = EDGE_CURVE ( 'NONE', #9781, #18611, #19613, .T. ) ;
#18402 = LINE ( 'NONE', #1247, #11329 ) ;
#18403 = ADVANCED_FACE ( 'NONE', ( #6790 ), #13618, .T. ) ;
#18404 = ORIENTED_EDGE ( 'NONE', *, *, #8012, .F. ) ;
#18405 = EDGE_CURVE ( 'NONE', #5100, #4633, #13819, .T. ) ;
#18406 = LINE ( 'NONE', #2362, #5520 ) ;
#18407 = CARTESIAN_POINT ( 'NONE',  ( 14.61823970408851459, -3577.393621464491389, 2249.830013958978725 ) ) ;
#18408 = DIRECTION ( 'NONE',  ( 0.000000000000000000, 1.000000000000000000, 0.000000000000000000 ) ) ;
#18409 = ORIENTED_EDGE ( 'NONE', *, *, #23119, .F. ) ;
#18411 = CARTESIAN_POINT ( 'NONE',  ( 137.9608668417556032, -3661.764029045890766, 2257.728452937817110 ) ) ;
#18410 = AXIS2_PLACEMENT_3D ( 'NONE', #11743, #15629, #13982 ) ;
#18412 = COORDINATED_UNIVERSAL_TIME_OFFSET ( 0, 0, .AHEAD. ) ;
#18413 = AXIS2_PLACEMENT_3D ( 'NONE', #4110, #9836, #6338 ) ;
#18414 = CARTESIAN_POINT ( 'NONE',  ( 9.855200508393229697, -3659.504999998446692, 2257.962940200992307 ) ) ;
#18415 = FACE_OUTER_BOUND ( 'NONE', #16444, .T. ) ;
#18416 = ORIENTED_EDGE ( 'NONE', *, *, #17435, .T. ) ;
#18417 = CARTESIAN_POINT ( 'NONE',  ( 20.52303563691415889, -3543.553571235837353, 2260.091479989294839 ) ) ;
#18418 = CARTESIAN_POINT ( 'NONE',  ( 139.6999999999999886, -3659.504999999999654, 2239.391000000000076 ) ) ;
#18419 = ADVANCED_FACE ( 'NONE', ( #15576, #12292 ), #11934, .T. ) ;
#18420 = ORIENTED_EDGE ( 'NONE', *, *, #14655, .T. ) ;
#18421 = VECTOR ( 'NONE', #7245, 1000.000000000000000 ) ;
#18422 = CARTESIAN_POINT ( 'NONE',  ( 140.4994326884994678, -3662.235235933393142, 2249.316303956256888 ) ) ;
#18423 = ORIENTED_EDGE ( 'NONE', *, *, #1065, .F. ) ;
#18424 = ORIENTED_EDGE ( 'NONE', *, *, #2007, .F. ) ;
#18425 = EDGE_LOOP ( 'NONE', ( #2322, #9440, #17363, #13564, #16957 ) ) ;
#18426 = AXIS2_PLACEMENT_3D ( 'NONE', #18966, #4239, #15332 ) ;
#18427 = VECTOR ( 'NONE', #202, 1000.000000000000000 ) ;
#18428 = CARTESIAN_POINT ( 'NONE',  ( 88.90000000000000568, -3644.899999999999636, 2260.600000000000364 ) ) ;
#18429 = ORIENTED_EDGE ( 'NONE', *, *, #371, .T. ) ;
#18430 = DIRECTION ( 'NONE',  ( 0.000000000000000000, 0.000000000000000000, 1.000000000000000000 ) ) ;
#18431 = DIRECTION ( 'NONE',  ( 1.000000000000000000, -2.334777064353000131E-14, -2.343004830739999973E-14 ) ) ;
#18432 = ORIENTED_EDGE ( 'NONE', *, *, #20041, .T. ) ;
#18433 = CARTESIAN_POINT ( 'NONE',  ( 7.117165288956338820, -3658.282806376657391, 2245.236545222771838 ) ) ;
#18434 = DIRECTION ( 'NONE',  ( 0.000000000000000000, -1.000000000000000000, 0.000000000000000000 ) ) ;
#18435 = CARTESIAN_POINT ( 'NONE',  ( 139.6999999999999886, -3659.504999999999654, 2239.771999999999935 ) ) ;
#18436 = DIRECTION ( 'NONE',  ( 0.000000000000000000, 1.000000000000000000, 0.000000000000000000 ) ) ;
#18437 = VECTOR ( 'NONE', #7302, 1000.000000000000000 ) ;
#18438 = CALENDAR_DATE ( 2026, 26, 10 ) ;
#18439 = EDGE_CURVE ( 'NONE', #17884, #20138, #12874, .T. ) ;
#18440 = EDGE_CURVE ( 'NONE', #12110, #15239, #4270, .T. ) ;
#18441 = CARTESIAN_POINT ( 'NONE',  ( 132.3005794017000198, -3694.430000000000291, 2260.390449568000349 ) ) ;
#18442 = TOROIDAL_SURFACE ( 'NONE', #7959, 3.606799999999999784, 0.7620000000000000107 ) ;
#18443 = AXIS2_PLACEMENT_3D ( 'NONE', #21244, #8700, #10685 ) ;
#18444 = DIRECTION ( 'NONE',  ( -1.000000000000000000, 0.000000000000000000, 0.000000000000000000 ) ) ;
#18445 = CARTESIAN_POINT ( 'NONE',  ( 15.24000000000000021, -3658.223872745999870, 2255.774000000000342 ) ) ;
#18446 = ADVANCED_FACE ( 'NONE', ( #21204 ), #5257, .T. ) ;
#18447 = ORIENTED_EDGE ( 'NONE', *, *, #8843, .F. ) ;
#18448 = DIRECTION ( 'NONE',  ( 0.000000000000000000, 0.000000000000000000, -1.000000000000000000 ) ) ;
#18449 = CARTESIAN_POINT ( 'NONE',  ( 0.7620000000000000107, -3695.699999999999818, 2295.829799999999977 ) ) ;
#18450 = EDGE_LOOP ( 'NONE', ( #6895, #18305, #5644, #1913, #13593, #20134, #14808, #16439 ) ) ;
#18451 = AXIS2_PLACEMENT_3D ( 'NONE', #17315, #12048, #8307 ) ;
#18452 = EDGE_CURVE ( 'NONE', #11171, #18027, #14384, .T. ) ;
#18453 = CARTESIAN_POINT ( 'NONE',  ( 139.8886820241594648, -3582.339796521665448, 2257.592643472502459 ) ) ;
#18454 = EDGE_CURVE ( 'NONE', #20632, #10769, #5778, .T. ) ;
#18455 = CARTESIAN_POINT ( 'NONE',  ( 18.36780534667559550, -3658.772087440082032, 2244.897599096027079 ) ) ;
#18456 = ORIENTED_EDGE ( 'NONE', *, *, #20113, .T. ) ;
#18457 = DIRECTION ( 'NONE',  ( 0.000000000000000000, 0.000000000000000000, -1.000000000000000000 ) ) ;
#18458 = CYLINDRICAL_SURFACE ( 'NONE', #7292, 5.715000000000997282 ) ;
#18459 = AXIS2_PLACEMENT_3D ( 'NONE', #18209, #12933, #3914 ) ;
#18460 = PLANE ( 'NONE',  #3953 ) ;
#18461 = VECTOR ( 'NONE', #12323, 1000.000000000000000 ) ;
#18462 = DIRECTION ( 'NONE',  ( 0.000000000000000000, 0.000000000000000000, 1.000000000000000000 ) ) ;
#18463 = CARTESIAN_POINT ( 'NONE',  ( 142.5174422324677153, -3543.437357047561363, 2255.079235783017793 ) ) ;
#18464 = LINE ( 'NONE', #16591, #11689 ) ;
#18465 = CARTESIAN_POINT ( 'NONE',  ( 7.497499966924064729, -3577.129409902275256, 2245.133902264068638 ) ) ;
#18466 = ORIENTED_EDGE ( 'NONE', *, *, #15229, .T. ) ;
#18467 = PERSON_AND_ORGANIZATION_ROLE ( 'design_supplier' ) ;
#18468 = ADVANCED_FACE ( 'NONE', ( #20268 ), #12404, .T. ) ;
#18469 = DIRECTION ( 'NONE',  ( -1.000000000000000000, 0.000000000000000000, 0.000000000000000000 ) ) ;
#18470 = AXIS2_PLACEMENT_3D ( 'NONE', #6787, #7553, #5147 ) ;
#18471 = CARTESIAN_POINT ( 'NONE',  ( 9.855390812759999619, -3579.528596999999991, 2250.157115725000040 ) ) ;
#18472 = LINE ( 'NONE', #20133, #21717 ) ;
#18473 = EDGE_LOOP ( 'NONE', ( #9162, #13088 ) ) ;
#18474 = CARTESIAN_POINT ( 'NONE',  ( 134.2617953917601028, -3661.301260524150166, 2244.777305218606216 ) ) ;
#18475 =( REPRESENTATION_RELATIONSHIP ('NONE','NONE', #20448, #18056 ) REPRESENTATION_RELATIONSHIP_WITH_TRANSFORMATION ( #3710 )SHAPE_REPRESENTATION_RELATIONSHIP( ) );
#18476 = VERTEX_POINT ( 'NONE', #6905 ) ;
#18477 = DIRECTION ( 'NONE',  ( 1.000000000000000000, 0.000000000000000000, 0.000000000000000000 ) ) ;
#18478 = ORIENTED_EDGE ( 'NONE', *, *, #16948, .F. ) ;
#18479 = CARTESIAN_POINT ( 'NONE',  ( 15.44120561128188562, -3660.278885126651858, 2250.236802488000194 ) ) ;
#18480 = LINE ( 'NONE', #12752, #15563 ) ;
#18481 = VERTEX_POINT ( 'NONE', #1386 ) ;
#18482 = SPHERICAL_SURFACE ( 'NONE', #3147, 1.270000000000000018 ) ;
#18483 = AXIS2_PLACEMENT_3D ( 'NONE', #18505, #6327, #13459 ) ;
#18484 = DIRECTION ( 'NONE',  ( 0.000000000000000000, 0.000000000000000000, 1.000000000000000000 ) ) ;
#18485 = ORIENTED_EDGE ( 'NONE', *, *, #4149, .T. ) ;
#18486 = DIRECTION ( 'NONE',  ( 0.000000000000000000, -1.000000000000000000, 0.000000000000000000 ) ) ;
#18487 = VECTOR ( 'NONE', #9669, 999.9999999999998863 ) ;
#18488 = DIRECTION ( 'NONE',  ( -1.000000000000000000, 0.000000000000000000, 0.000000000000000000 ) ) ;
#18489 = ORIENTED_EDGE ( 'NONE', *, *, #10783, .F. ) ;
#18490 = B_SPLINE_CURVE_WITH_KNOTS ( 'NONE', 3,
 ( #1891, #21591, #5547, #21357, #26, #19595, #9044, #12561, #16195, #12677, #14561, #3758, #3883, #21814, #10915, #3529, #18065 ),
 .UNSPECIFIED., .F., .F.,
 ( 4, 1, 1, 1, 1, 1, 1, 1, 1, 1, 1, 1, 1, 1, 4 ),
 ( 0.000000000000000000, 0.07142857142856999519, 0.1428571428570999946, 0.2142857142857000075, 0.2857142857143000203, 0.3571428571429000054, 0.4285714285713999594, 0.5000000000000000000, 0.5714285714286000406, 0.6428571428570999391, 0.7142857142856999797, 0.7857142857142999093, 0.8571428571429000609, 0.9285714285714000704, 1.000000000000000000 ),
 .UNSPECIFIED. ) ;
#18491 = EDGE_LOOP ( 'NONE', ( #11217, #727, #18825, #21260 ) ) ;
#18492 = DIRECTION ( 'NONE',  ( 0.000000000000000000, 0.000000000000000000, -1.000000000000000000 ) ) ;
#18493 = ORIENTED_EDGE ( 'NONE', *, *, #14392, .T. ) ;
#18494 = DIRECTION ( 'NONE',  ( 0.000000000000000000, 1.000000000000000000, 0.000000000000000000 ) ) ;
#18495 = CALENDAR_DATE ( 2026, 26, 10 ) ;
#18496 = PRODUCT_RELATED_PRODUCT_CATEGORY ( 'detail', '', ( #20975 ) ) ;
#18497 = CARTESIAN_POINT ( 'NONE',  ( 15.53321004273999861, -3639.816849713999545, 2279.450415087999772 ) ) ;
#18498 = CARTESIAN_POINT ( 'NONE',  ( 17.60812544259881562, -3662.432924330847982, 2245.707771157191928 ) ) ;
#18499 = B_SPLINE_CURVE_WITH_KNOTS ( 'NONE', 3,
 ( #18471, #2425, #8040, #13542, #21987, #2754, #13425, #666, #22094, #4631, #18930, #9458, #549, #1462, #12256, #8621, #10373, #12366, #14015, #1110, #11903, #22671, #15887, #21283, #23018, #8741, #4989, #3106, #19052, #17631, #6645, #15535, #17515, #8272, #21165, #10488, #17392, #15770, #22782, #10254, #5112, #1348, #1583, #12130, #1229, #6524, #10026, #12018, #20806, #6992, #17166, #14135, #22899, #13784, #13660, #5227, #2881, #19287, #20926, #15421, #22554, #3227, #4754, #3336, #6755, #2991 ),
 .UNSPECIFIED., .F., .F.,
 ( 4, 2, 1, 1, 2, 2, 2, 1, 1, 2, 2, 2, 2, 1, 1, 1, 1, 2, 2, 2, 2, 1, 2, 2, 2, 2, 1, 2, 2, 2, 2, 2, 2, 2, 2, 2, 2, 4 ),
 ( 0.000000000000000000, 0.06250000001292387031, 0.09375000001938579852, 0.1093750000227409619, 0.1171875000244185505, 0.1250000000260961253, 0.1875000000388516719, 0.2187500000451599591, 0.2343750000483139639, 0.2421875000498185937, 0.2500000000513232234, 0.3125000000629582497, 0.3437500000687803703, 0.3593750000717660931, 0.3671875000732587879, 0.3710937500739424078, 0.3730468750743454742, 0.3740234375744863615, 0.3750000000746271933, 0.4062500000718055060, 0.4218750000703743175, 0.4296875000695432045, 0.4335937500691276481, 0.4375000000687120916, 0.4687500000660348998, 0.4843750000646543930, 0.4921875000640169029, 0.4960937500635165254, 0.5000000000630161479, 0.5625000000558735280, 0.5937500000522591970, 0.6093750000502783370, 0.6250000000482974771, 0.6875000000403100886, 0.7500000000323225890, 0.8125000000243352005, 0.8750000000163478120, 1.000000000000000000 ),
 .UNSPECIFIED. ) ;
#18500 = AXIS2_PLACEMENT_3D ( 'NONE', #22560, #10146, #11908 ) ;
#18501 = CARTESIAN_POINT ( 'NONE',  ( 95.25000000000000000, -3568.700000000000273, 2247.392000000000280 ) ) ;
#18502 = DIRECTION ( 'NONE',  ( -0.000000000000000000, -0.000000000000000000, 1.000000000000000000 ) ) ;
#18503 = ADVANCED_FACE ( 'NONE', ( #4903 ), #8020, .T. ) ;
#18504 = CIRCLE ( 'NONE', #8408, 2.844800000000091700 ) ;
#18505 = CARTESIAN_POINT ( 'NONE',  ( 0.7620000000000000107, -3694.938000000000102, 2295.829799999999977 ) ) ;
#18506 = ORIENTED_EDGE ( 'NONE', *, *, #2776, .T. ) ;
#18507 = DIRECTION ( 'NONE',  ( 0.000000000000000000, 0.000000000000000000, -1.000000000000000000 ) ) ;
#18508 = VERTEX_POINT ( 'NONE', #12050 ) ;
#18509 = CARTESIAN_POINT ( 'NONE',  ( 136.8551999999999964, -3579.494999999999891, 2256.063560000000052 ) ) ;
#18510 = VERTEX_POINT ( 'NONE', #15924 ) ;
#18511 = CARTESIAN_POINT ( 'NONE',  ( 13.92841025336000094, -3596.924928188000194, 2279.750815200000034 ) ) ;
#18512 = CARTESIAN_POINT ( 'NONE',  ( 15.74707948048999917, -3543.299999999999727, 2254.503999999999905 ) ) ;
#18513 = ORIENTED_EDGE ( 'NONE', *, *, #4140, .F. ) ;
#18514 = ORIENTED_EDGE ( 'NONE', *, *, #8874, .F. ) ;
#18515 = FACE_OUTER_BOUND ( 'NONE', #16722, .T. ) ;
#18516 = TOROIDAL_SURFACE ( 'NONE', #13708, 3.606799999999999784, 0.7620000000000000107 ) ;
#18517 = TOROIDAL_SURFACE ( 'NONE', #6185, 5.080000000000000071, 0.3810000000000000053 ) ;
#18518 = EDGE_LOOP ( 'NONE', ( #7634, #7096, #19870, #10910 ) ) ;
#18519 = AXIS2_PLACEMENT_3D ( 'NONE', #18980, #18627, #6218 ) ;
#18520 = CARTESIAN_POINT ( 'NONE',  ( -5.588000000000000078, -3578.860000000000127, 2250.998800000000301 ) ) ;
#18521 = CARTESIAN_POINT ( 'NONE',  ( 14.46426801451776356, -3577.263211980953201, 2249.746456749269782 ) ) ;
#18522 = TOROIDAL_SURFACE ( 'NONE', #16645, 6.477000000000000313, 0.7620000000000000107 ) ;
#18523 = CARTESIAN_POINT ( 'NONE',  ( 142.0852733101186516, -3581.045180569711192, 2249.213504086232206 ) ) ;
#18524 = ORIENTED_EDGE ( 'NONE', *, *, #17533, .T. ) ;
#18525 = DIRECTION ( 'NONE',  ( 0.000000000000000000, -1.000000000000000000, 0.000000000000000000 ) ) ;
#18526 = PERSON_AND_ORGANIZATION ( #5446, #1895 ) ;
#18527 = APPLIED_DATE_AND_TIME_ASSIGNMENT ( #3916, #5576, ( #6402 ) ) ;
#18528 = CARTESIAN_POINT ( 'NONE',  ( 20.53015567188813861, -3543.540473573110376, 2260.073663966102231 ) ) ;
#18529 = FACE_OUTER_BOUND ( 'NONE', #42, .T. ) ;
#18530 = ADVANCED_FACE ( 'NONE', ( #19206 ), #19552, .F. ) ;
#18531 = ADVANCED_FACE ( 'NONE', ( #14051 ), #10171, .F. ) ;
#18532 = TOROIDAL_SURFACE ( 'NONE', #215, 6.477000000000000313, 0.7620000000000000107 ) ;
#18533 = VERTEX_POINT ( 'NONE', #17317 ) ;
#18534 = VECTOR ( 'NONE', #4671, 1000.000000000000114 ) ;
#18535 = CARTESIAN_POINT ( 'NONE',  ( 101.5999999999999943, -3670.300000000000182, 2239.771999999999935 ) ) ;
#18537 = ADVANCED_FACE ( 'NONE', ( #22818 ), #3902, .T. ) ;
#18536 = VECTOR ( 'NONE', #16832, 1000.000000000000000 ) ;
#18538 = ORIENTED_EDGE ( 'NONE', *, *, #8221, .T. ) ;
#18539 = ORIENTED_EDGE ( 'NONE', *, *, #21400, .F. ) ;
#18540 = DIRECTION ( 'NONE',  ( 0.000000000000000000, 1.000000000000000000, 0.000000000000000000 ) ) ;
#18541 = EDGE_LOOP ( 'NONE', ( #20857, #7085, #21489, #256 ) ) ;
#18542 = CARTESIAN_POINT ( 'NONE',  ( 114.2999999999999972, -3594.099999999999909, 2239.009999999999764 ) ) ;
#18543 = CARTESIAN_POINT ( 'NONE',  ( 12.70000000023389042, -3642.634840905157944, 2296.591799999999694 ) ) ;
#18544 = ORIENTED_EDGE ( 'NONE', *, *, #22817, .F. ) ;
#18545 = CARTESIAN_POINT ( 'NONE',  ( 7.200432652932446054, -3657.950405511532608, 2245.575309129941616 ) ) ;
#18546 = PLANE ( 'NONE',  #7471 ) ;
#18547 = CYLINDRICAL_SURFACE ( 'NONE', #8735, 0.3809999999999993947 ) ;
#18548 = EDGE_CURVE ( 'NONE', #5448, #5087, #17548, .T. ) ;
#18549 = AXIS2_PLACEMENT_3D ( 'NONE', #1649, #22000, #18484 ) ;
#18550 = AXIS2_PLACEMENT_3D ( 'NONE', #15088, #18824, #10035 ) ;
#18551 = CYLINDRICAL_SURFACE ( 'NONE', #10351, 0.7619999999999996776 ) ;
#18552 = PERSON_AND_ORGANIZATION_ROLE ( 'design_supplier' ) ;
#18553 = AXIS2_PLACEMENT_3D ( 'NONE', #21313, #9120, #19786 ) ;
#18554 = CIRCLE ( 'NONE', #14822, 2.844800000000001550 ) ;
#18555 = CYLINDRICAL_SURFACE ( 'NONE', #16894, 2.844799999999994444 ) ;
#18556 = AXIS2_PLACEMENT_3D ( 'NONE', #8862, #15893, #12371 ) ;
#18557 = CARTESIAN_POINT ( 'NONE',  ( 127.0000000000000000, -3619.500000000000000, 2239.771999999999935 ) ) ;
#18558 = FACE_OUTER_BOUND ( 'NONE', #4552, .T. ) ;
#18559 = AXIS2_PLACEMENT_3D ( 'NONE', #6116, #13242, #10420 ) ;
#18560 = ORIENTED_EDGE ( 'NONE', *, *, #11946, .F. ) ;
#18561 = DIRECTION ( 'NONE',  ( 0.000000000000000000, -1.000000000000000000, 0.000000000000000000 ) ) ;
#18562 = EDGE_CURVE ( 'NONE', #11737, #18679, #22957, .T. ) ;
#18563 = CIRCLE ( 'NONE', #13334, 2.844799999999994444 ) ;
#18564 = FACE_OUTER_BOUND ( 'NONE', #1292, .T. ) ;
#18565 = ORIENTED_EDGE ( 'NONE', *, *, #19464, .F. ) ;
#18566 = DIRECTION ( 'NONE',  ( 1.000000000000000000, 0.000000000000000000, 0.000000000000000000 ) ) ;
#18567 = EDGE_CURVE ( 'NONE', #5595, #650, #3144, .T. ) ;
#18568 = AXIS2_PLACEMENT_3D ( 'NONE', #22590, #4332, #8194 ) ;
#18569 = ADVANCED_FACE ( 'NONE', ( #20021 ), #21428, .T. ) ;
#18570 = DIRECTION ( 'NONE',  ( -1.000000000000000000, 0.000000000000000000, 0.000000000000000000 ) ) ;
#18571 = ORIENTED_EDGE ( 'NONE', *, *, #1034, .F. ) ;
#18572 = ORIENTED_EDGE ( 'NONE', *, *, #1531, .F. ) ;
#18573 = DIRECTION ( 'NONE',  ( 1.000000000000000000, 0.000000000000000000, 0.000000000000000000 ) ) ;
#18574 = CARTESIAN_POINT ( 'NONE',  ( 95.24999999999970157, -3670.300000000000182, 2244.547199999999975 ) ) ;
#18575 = AXIS2_PLACEMENT_3D ( 'NONE', #22645, #13284, #11525 ) ;
#18576 = DIRECTION ( 'NONE',  ( 0.000000000000000000, -1.000000000000000000, 0.000000000000000000 ) ) ;
#18577 = TOROIDAL_SURFACE ( 'NONE', #3239, 3.606799999998999695, 0.7620000000000000107 ) ;
#18578 = DIRECTION ( 'NONE',  ( 0.000000000000000000, 0.000000000000000000, 1.000000000000000000 ) ) ;
#18579 = CARTESIAN_POINT ( 'NONE',  ( 142.5447999999993272, -3579.043785370568457, 2256.063560000000962 ) ) ;
#18580 = FACE_OUTER_BOUND ( 'NONE', #14903, .T. ) ;
#18581 = CARTESIAN_POINT ( 'NONE',  ( 20.70551549691483828, -3695.663357297210496, 2259.634152369406365 ) ) ;
#18582 = VERTEX_POINT ( 'NONE', #1974 ) ;
#18583 = CALENDAR_DATE ( 2026, 26, 10 ) ;
#18584 = EDGE_LOOP ( 'NONE', ( #420, #13177, #19424, #10151 ) ) ;
#18585 = FACE_OUTER_BOUND ( 'NONE', #20188, .T. ) ;
#18586 = ADVANCED_FACE ( 'NONE', ( #9125 ), #7368, .F. ) ;
#18587 = FACE_BOUND ( 'NONE', #6070, .T. ) ;
#18588 = VECTOR ( 'NONE', #3305, 1000.000000000000000 ) ;
#18589 = CARTESIAN_POINT ( 'NONE',  ( 137.3683132029000262, -3578.148799999999937, 2242.820000000000164 ) ) ;
#18590 = VERTEX_POINT ( 'NONE', #12868 ) ;
#18591 = CARTESIAN_POINT ( 'NONE',  ( 134.7212531515910996, -3662.318798419799805, 2245.535362107170840 ) ) ;
#18592 = CIRCLE ( 'NONE', #9989, 0.7619999999999294005 ) ;
#18593 = CARTESIAN_POINT ( 'NONE',  ( 12.69999999999999929, -3639.502500000000055, 2288.971800000000258 ) ) ;
#18594 = EDGE_LOOP ( 'NONE', ( #13014, #19030 ) ) ;
#18595 = CARTESIAN_POINT ( 'NONE',  ( 20.32000000000000028, -3544.061999999999898, 2289.213099999999940 ) ) ;
#18596 = CARTESIAN_POINT ( 'NONE',  ( 13.16106602307787732, -3662.312985057125843, 2249.228091833082544 ) ) ;
#18597 = EDGE_CURVE ( 'NONE', #9312, #6119, #16988, .T. ) ;
#18598 = DIRECTION ( 'NONE',  ( 2.336881798971000105E-14, 2.336881798971000105E-14, 1.000000000000000000 ) ) ;
#18599 = ORIENTED_EDGE ( 'NONE', *, *, #8712, .T. ) ;
#18600 = DIRECTION ( 'NONE',  ( 1.000000000000000000, 0.000000000000000000, 0.000000000000000000 ) ) ;
#18601 = CARTESIAN_POINT ( 'NONE',  ( 38.10000000000000142, -3644.899999999999636, 2259.837999999999738 ) ) ;
#18602 = VECTOR ( 'NONE', #15020, 1000.000000000000000 ) ;
#18603 = DIRECTION ( 'NONE',  ( -2.334777064352623371E-14, -1.000000000000000000, 0.000000000000000000 ) ) ;
#18604 = CARTESIAN_POINT ( 'NONE',  ( 9.855199999999999960, -3639.502500000000055, 2263.571799999999712 ) ) ;
#18605 = ORIENTED_EDGE ( 'NONE', *, *, #693, .F. ) ;
#18606 = VERTEX_POINT ( 'NONE', #19789 ) ;
#18607 = VECTOR ( 'NONE', #14517, 1000.000000000000000 ) ;
#18608 = CIRCLE ( 'NONE', #13753, 3.175000000000149925 ) ;
#18609 = CARTESIAN_POINT ( 'NONE',  ( 12.69999999999999929, -3659.504999999999654, 2272.030000000000200 ) ) ;
#18610 = CIRCLE ( 'NONE', #14085, 3.606799999999993567 ) ;
#18611 = VERTEX_POINT ( 'NONE', #2095 ) ;
#18612 = ADVANCED_FACE ( 'NONE', ( #4072 ), #14753, .T. ) ;
#18613 = CARTESIAN_POINT ( 'NONE',  ( 145.2625040556375211, -3580.806353043091349, 2245.317242612459722 ) ) ;
#18614 = PERSON_AND_ORGANIZATION_ROLE ( 'classification_officer' ) ;
#18615 = ADVANCED_FACE ( 'NONE', ( #16264, #2207 ), #16381, .F. ) ;
#18616 = CARTESIAN_POINT ( 'NONE',  ( 12.69999999999999929, -3654.043999999999869, 2245.359999999999673 ) ) ;
#18617 = CARTESIAN_POINT ( 'NONE',  ( 18.36256270591483286, -3660.286495684446891, 2244.547215521768521 ) ) ;
#18618 = CARTESIAN_POINT ( 'NONE',  ( 15.54479972196000048, -3579.494985918000111, 2257.962943248000101 ) ) ;
#18619 = DIRECTION ( 'NONE',  ( 0.000000000000000000, 0.000000000000000000, 1.000000000000000000 ) ) ;
#18620 = CIRCLE ( 'NONE', #16018, 3.175000000000149925 ) ;
#18621 = DIRECTION ( 'NONE',  ( 0.000000000000000000, 0.000000000000000000, 1.000000000000000000 ) ) ;
#18622 = VERTEX_POINT ( 'NONE', #18023 ) ;
#18623 = CARTESIAN_POINT ( 'NONE',  ( 12.69999999999999929, -3599.497499999999945, 2290.241799999999785 ) ) ;
#18624 = AXIS2_PLACEMENT_3D ( 'NONE', #17023, #737, #2615 ) ;
#18625 = CARTESIAN_POINT ( 'NONE',  ( 0.000000000000000000, -3660.140000000000327, 2247.392000000000280 ) ) ;
#18626 = ORIENTED_EDGE ( 'NONE', *, *, #10893, .F. ) ;
#18627 = DIRECTION ( 'NONE',  ( 0.000000000000000000, 0.5000000000031962211, -0.8660254037825932949 ) ) ;
#18628 = CARTESIAN_POINT ( 'NONE',  ( 141.4351164976492612, -3661.767009749791214, 2257.727830822052056 ) ) ;
#18629 = ORIENTED_EDGE ( 'NONE', *, *, #9235, .F. ) ;
#18630 = ORIENTED_EDGE ( 'NONE', *, *, #2351, .T. ) ;
#18631 = ORIENTED_EDGE ( 'NONE', *, *, #14152, .F. ) ;
#18632 = PLANE ( 'NONE',  #18769 ) ;
#18633 = ORIENTED_EDGE ( 'NONE', *, *, #17070, .T. ) ;
#18634 = AXIS2_PLACEMENT_3D ( 'NONE', #15389, #18898, #6266 ) ;
#18635 = CARTESIAN_POINT ( 'NONE',  ( 12.69999999999999929, -3644.963499999999840, 2290.622800000000097 ) ) ;
#18636 = CARTESIAN_POINT ( 'NONE',  ( 12.43234888807521976, -3576.659528385393969, 2249.195257278045574 ) ) ;
#18637 = DIRECTION ( 'NONE',  ( 0.000000000000000000, 0.000000000000000000, 1.000000000000000000 ) ) ;
#18638 = CARTESIAN_POINT ( 'NONE',  ( 141.8494091026127819, -3581.358993298141741, 2248.752437981420371 ) ) ;
#18639 = ORIENTED_EDGE ( 'NONE', *, *, #5372, .F. ) ;
#18640 = CARTESIAN_POINT ( 'NONE',  ( 138.9568794923274595, -3662.257434252253006, 2257.615983646263885 ) ) ;
#18641 = APPROVAL_STATUS ( 'not_yet_approved' ) ;
#18642 = CARTESIAN_POINT ( 'NONE',  ( 12.69998491500983206, -3602.342301254179802, 2279.817638609000369 ) ) ;
#18643 = B_SPLINE_CURVE_WITH_KNOTS ( 'NONE', 3,
 ( #20698, #13558, #11796, #11916, #17063, #2771, #19064, #9803, #6192, #15552, #9694, #20580, #6539, #18948, #9914, #8287, #20827 ),
 .UNSPECIFIED., .F., .F.,
 ( 4, 1, 1, 1, 1, 1, 1, 1, 1, 1, 1, 1, 1, 1, 4 ),
 ( 5.006989800018624494E-06, 0.07142857142856999519, 0.1428571428570999946, 0.2142857142857000075, 0.2857142857143000203, 0.3571428571429000054, 0.4285714285713999594, 0.5000000000000000000, 0.5714285714286000406, 0.6428571428570999391, 0.7142857142856999797, 0.7857142857142999093, 0.8571428571429000609, 0.9285714285714000704, 1.000000000000000000 ),
 .UNSPECIFIED. ) ;
#18644 = PLANE ( 'NONE',  #2547 ) ;
#18645 = CARTESIAN_POINT ( 'NONE',  ( -12.31899999999998663, -3662.832400000169400, 2247.392000000001190 ) ) ;
#18646 = ORIENTED_EDGE ( 'NONE', *, *, #16559, .F. ) ;
#18647 = FACE_OUTER_BOUND ( 'NONE', #13240, .T. ) ;
#18648 = EDGE_LOOP ( 'NONE', ( #614, #10280, #15129, #11675, #15633, #12989, #21496, #8341 ) ) ;
#18649 = AXIS2_PLACEMENT_3D ( 'NONE', #20828, #4771, #2897 ) ;
#18650 = ORIENTED_EDGE ( 'NONE', *, *, #11096, .F. ) ;
#18651 = APPROVAL ( #16198, 'UNSPECIFIED' ) ;
#18652 = LINE ( 'NONE', #22389, #8442 ) ;
#18653 = EDGE_CURVE ( 'NONE', #15991, #2058, #17906, .T. ) ;
#18654 = EDGE_LOOP ( 'NONE', ( #4043, #8904, #1721, #5181 ) ) ;
#18655 = DIRECTION ( 'NONE',  ( -1.000000000000000000, 0.000000000000000000, 0.000000000000000000 ) ) ;
#18656 = DIRECTION ( 'NONE',  ( 1.097617497454356000E-13, 0.000000000000000000, 1.000000000000000000 ) ) ;
#18657 = VERTEX_POINT ( 'NONE', #3606 ) ;
#18658 = CARTESIAN_POINT ( 'NONE',  ( 7.015536193038670376, -3658.914394104701387, 2244.824399554300726 ) ) ;
#18659 = EDGE_CURVE ( 'NONE', #22036, #15032, #12749, .T. ) ;
#18660 = DIRECTION ( 'NONE',  ( 0.000000000000000000, 0.000000000000000000, -1.000000000000000000 ) ) ;
#18661 = ADVANCED_FACE ( 'NONE', ( #10875 ), #5614, .T. ) ;
#18662 = DIRECTION ( 'NONE',  ( 0.000000000000000000, -1.000000000000000000, 0.000000000000000000 ) ) ;
#18663 = CALENDAR_DATE ( 2026, 26, 10 ) ;
#18664 = ADVANCED_FACE ( 'NONE', ( #2317 ), #9463, .T. ) ;
#18665 = PLANE ( 'NONE',  #15789 ) ;
#18666 = LINE ( 'NONE', #4063, #14155 ) ;
#18667 = CIRCLE ( 'NONE', #2963, 6.349999999999855760 ) ;
#18668 = CARTESIAN_POINT ( 'NONE',  ( 142.4126867972000241, -3657.938829547000296, 2239.009999999999764 ) ) ;
#18669 = DIRECTION ( 'NONE',  ( 0.000000000000000000, 0.000000000000000000, 1.000000000000000000 ) ) ;
#18670 = EDGE_CURVE ( 'NONE', #19756, #22778, #5790, .T. ) ;
#18671 = ORIENTED_EDGE ( 'NONE', *, *, #132, .T. ) ;
#18672 = CARTESIAN_POINT ( 'NONE',  ( 137.0197613996714381, -3543.693183278374363, 2255.422803182008920 ) ) ;
#18673 = EDGE_CURVE ( 'NONE', #8713, #9808, #14028, .T. ) ;
#18674 = ORIENTED_EDGE ( 'NONE', *, *, #7737, .F. ) ;
#18675 = CARTESIAN_POINT ( 'NONE',  ( 139.6999999999999886, -3659.504999999999654, 2239.009999999999764 ) ) ;
#18676 = ADVANCED_FACE ( 'NONE', ( #5503 ), #9519, .T. ) ;
#18677 = CARTESIAN_POINT ( 'NONE',  ( 12.69999999999999929, -3582.670000000000073, 2270.760000000000218 ) ) ;
#18678 = ORIENTED_EDGE ( 'NONE', *, *, #10558, .T. ) ;
#18679 = VERTEX_POINT ( 'NONE', #20242 ) ;
#18680 = LINE ( 'NONE', #11757, #7896 ) ;
#18681 = CARTESIAN_POINT ( 'NONE',  ( 18.37960467573999779, -3578.859731361000286, 2244.547525601999951 ) ) ;
#18682 = CARTESIAN_POINT ( 'NONE',  ( 9.855201422231997910, -3599.602849033000439, 2279.447341858000073 ) ) ;
#18683 = FACE_OUTER_BOUND ( 'NONE', #17264, .T. ) ;
#18684 = DIRECTION ( 'NONE',  ( -1.000000000000000000, 0.000000000000000000, 0.000000000000000000 ) ) ;
#18685 = DIRECTION ( 'NONE',  ( 0.000000000000000000, 0.000000000000000000, -1.000000000000000000 ) ) ;
#18686 = ADVANCED_FACE ( 'NONE', ( #2761 ), #13632, .T. ) ;
#18687 = EDGE_LOOP ( 'NONE', ( #3412, #7714, #5881, #19113 ) ) ;
#18688 = DATE_AND_TIME ( #20458, #9012 ) ;
#18689 = EDGE_CURVE ( 'NONE', #16281, #15707, #21509, .T. ) ;
#18690 = CARTESIAN_POINT ( 'NONE',  ( -8.890000000022000748, -3661.486200000000281, 2245.060313203000078 ) ) ;
#18691 = AXIS2_PLACEMENT_3D ( 'NONE', #3862, #19922, #5978 ) ;
#18692 = CARTESIAN_POINT ( 'NONE',  ( 127.0000000000000000, -3660.140000000000327, 2247.392000000000280 ) ) ;
#18693 = DIRECTION ( 'NONE',  ( 0.000000000000000000, 0.000000000000000000, 1.000000000000000000 ) ) ;
#18694 = LOCAL_TIME ( 17, 37, 43.00000000000000000, #22516 ) ;
#18695 = ORIENTED_EDGE ( 'NONE', *, *, #17795, .F. ) ;
#18696 = CARTESIAN_POINT ( 'NONE',  ( 12.69999999997562057, -3602.189900000083526, 2296.210799999999836 ) ) ;
#18697 = EDGE_CURVE ( 'NONE', #13805, #13091, #6090, .T. ) ;
#18698 = CARTESIAN_POINT ( 'NONE',  ( 53.64479999999999649, -3619.500000000000000, 2239.771999999999935 ) ) ;
#18699 = DIRECTION ( 'NONE',  ( 0.000000000000000000, -1.000000000000000000, 0.000000000000000000 ) ) ;
#18700 = ORIENTED_EDGE ( 'NONE', *, *, #3073, .T. ) ;
#18701 = DIRECTION ( 'NONE',  ( 0.000000000000000000, 0.000000000000000000, -1.000000000000000000 ) ) ;
#18702 = CARTESIAN_POINT ( 'NONE',  ( 15.09589954392630595, -3661.040808043710513, 2250.091324297367009 ) ) ;
#18703 = DIRECTION ( 'NONE',  ( 0.000000000000000000, 0.000000000000000000, -1.000000000000000000 ) ) ;
#18704 = EDGE_LOOP ( 'NONE', ( #13382, #12344, #13140, #14583 ) ) ;
#18705 = LINE ( 'NONE', #15206, #18536 ) ;
#18706 = CYLINDRICAL_SURFACE ( 'NONE', #12934, 5.460999999999938126 ) ;
#18707 = DIRECTION ( 'NONE',  ( -2.324635735433000053E-14, 0.000000000000000000, -1.000000000000000000 ) ) ;
#18708 = CARTESIAN_POINT ( 'NONE',  ( 10.36831320284000135, -3598.151299999999992, 2296.210799999999836 ) ) ;
#18709 = LOCAL_TIME ( 17, 37, 43.00000000000000000, #20155 ) ;
#18710 = ORIENTED_EDGE ( 'NONE', *, *, #3357, .T. ) ;
#18711 = AXIS2_PLACEMENT_3D ( 'NONE', #11951, #10188, #13719 ) ;
#18712 = VERTEX_POINT ( 'NONE', #4636 ) ;
#18713 = CARTESIAN_POINT ( 'NONE',  ( 5.080000000000000071, -3544.570000000000164, 2260.600000000000364 ) ) ;
#18714 = VERTEX_POINT ( 'NONE', #4301 ) ;
#18715 = CARTESIAN_POINT ( 'NONE',  ( 12.69999999999999929, -3599.497499999999945, 2263.571799999999712 ) ) ;
#18716 = PERSON_AND_ORGANIZATION ( #19132, #18723 ) ;
#18717 = EDGE_CURVE ( 'NONE', #8155, #10930, #5957, .T. ) ;
#18718 = FACE_OUTER_BOUND ( 'NONE', #13544, .T. ) ;
#18719 = ADVANCED_FACE ( 'NONE', ( #9686 ), #4414, .F. ) ;
#18720 = CARTESIAN_POINT ( 'NONE',  ( 17.66446110557347637, -3662.336897614723057, 2245.582878452307796 ) ) ;
#18721 = CARTESIAN_POINT ( 'NONE',  ( -5.588000000000000078, -3660.140000000000327, 2247.392000000000280 ) ) ;
#18722 = DIRECTION ( 'NONE',  ( 3.283276570194000329E-13, 2.590196616239000129E-13, 1.000000000000000000 ) ) ;
#18723 = ORGANIZATION ( 'NAUO-ORG4', 'UNSPECIFIED', 'UNSPECIFIED' ) ;
#18724 = CARTESIAN_POINT ( 'NONE',  ( 4.572920519510000226, -3543.299999999999727, 2259.329999999999927 ) ) ;
#18725 = ADVANCED_FACE ( 'NONE', ( #4522 ), #11549, .T. ) ;
#18726 = ORIENTED_EDGE ( 'NONE', *, *, #21406, .T. ) ;
#18727 = APPROVAL_PERSON_ORGANIZATION ( #22832, #16097, #22950 ) ;
#18728 = DIRECTION ( 'NONE',  ( -1.000000000000000000, 0.000000000000000000, 0.000000000000000000 ) ) ;
#18729 = CARTESIAN_POINT ( 'NONE',  ( 114.2999999999999972, -3594.099999999999909, 2261.869999999999891 ) ) ;
#18730 = ORIENTED_EDGE ( 'NONE', *, *, #13869, .F. ) ;
#18731 = LINE ( 'NONE', #15003, #18153 ) ;
#18732 = CARTESIAN_POINT ( 'NONE',  ( 15.44174945842176250, -3543.555041883176273, 2255.268480148888102 ) ) ;
#18733 = EDGE_CURVE ( 'NONE', #6015, #825, #905, .T. ) ;
#18734 = VERTEX_POINT ( 'NONE', #18698 ) ;
#18735 = AXIS2_PLACEMENT_3D ( 'NONE', #14351, #9189, #21615 ) ;
#18736 = EDGE_CURVE ( 'NONE', #3892, #15432, #11442, .T. ) ;
#18737 = EDGE_LOOP ( 'NONE', ( #17208, #16465, #5322 ) ) ;
#18738 = DATE_TIME_ROLE ( 'classification_date' ) ;
#18739 = DIRECTION ( 'NONE',  ( 0.000000000000000000, 0.000000000000000000, -1.000000000000000000 ) ) ;
#18740 = EDGE_LOOP ( 'NONE', ( #17326, #6225, #14772 ) ) ;
#18741 = ORIENTED_EDGE ( 'NONE', *, *, #18178, .T. ) ;
#18742 = CARTESIAN_POINT ( 'NONE',  ( 50.79999999999999716, -3619.500000000000000, 2239.771999999999935 ) ) ;
#18743 = CARTESIAN_POINT ( 'NONE',  ( 11.08675752506961132, -3577.151045551118386, 2249.666716971718870 ) ) ;
#18744 = DIRECTION ( 'NONE',  ( 1.000000000000000000, 0.000000000000000000, 0.000000000000000000 ) ) ;
#18745 = ORGANIZATION ( 'NAUO-ORG12', 'UNSPECIFIED', 'UNSPECIFIED' ) ;
#18746 = CARTESIAN_POINT ( 'NONE',  ( 142.4841666229198722, -3580.081058733761438, 2249.961449664135216 ) ) ;
#18747 = ORIENTED_EDGE ( 'NONE', *, *, #1892, .T. ) ;
#18748 = CARTESIAN_POINT ( 'NONE',  ( 136.9464494524225984, -3660.243491359982727, 2257.939127531997201 ) ) ;
#18749 = APPROVAL_DATE_TIME ( #15250, #8051 ) ;
#18750 = ADVANCED_FACE ( 'NONE', ( #6181, #6302 ), #13429, .F. ) ;
#18751 = CARTESIAN_POINT ( 'NONE',  ( 20.32000000000000028, -3695.699999999999818, 2285.606299999999919 ) ) ;
#18752 = CARTESIAN_POINT ( 'NONE',  ( 20.67266563390785095, -3543.360310295285217, 2259.716802593130069 ) ) ;
#18753 = AXIS2_PLACEMENT_3D ( 'NONE', #17513, #6521, #6643 ) ;
#18754 = PRODUCT_DEFINITION_SHAPE ( 'NONE', 'NONE',  #23173 ) ;
#18755 = CARTESIAN_POINT ( 'NONE',  ( 15.54479999999999862, -3639.502500000000055, 2279.447335734999797 ) ) ;
#18756 = AXIS2_PLACEMENT_3D ( 'NONE', #14580, #18203, #4027 ) ;
#18757 = ORIENTED_EDGE ( 'NONE', *, *, #14688, .F. ) ;
#18758 = CARTESIAN_POINT ( 'NONE',  ( -12.69999999999999929, -3577.293829546977122, 2244.679313203000220 ) ) ;
#18759 = ORIENTED_EDGE ( 'NONE', *, *, #7220, .T. ) ;
#18760 = ORIENTED_EDGE ( 'NONE', *, *, #2896, .F. ) ;
#18761 = EDGE_LOOP ( 'NONE', ( #5268, #286 ) ) ;
#18762 = CARTESIAN_POINT ( 'NONE',  ( 53.64479999999999649, -3568.700000000000273, 2259.837999999999738 ) ) ;
#18763 = ORIENTED_EDGE ( 'NONE', *, *, #14749, .T. ) ;
#18764 = EDGE_LOOP ( 'NONE', ( #15036, #21215 ) ) ;
#18765 = DIRECTION ( 'NONE',  ( 1.000000000000000000, 0.000000000000000000, 0.000000000000000000 ) ) ;
#18766 = CARTESIAN_POINT ( 'NONE',  ( 12.69999999999999929, -3659.504999999999654, 2246.630000000000109 ) ) ;
#18767 = AXIS2_PLACEMENT_3D ( 'NONE', #22179, #12940, #15046 ) ;
#18768 = EDGE_LOOP ( 'NONE', ( #1816, #9187, #19790, #11922 ) ) ;
#18769 = AXIS2_PLACEMENT_3D ( 'NONE', #18400, #20389, #2357 ) ;
#18770 = CARTESIAN_POINT ( 'NONE',  ( 6.985153502415999860, -3659.505556594000154, 2244.618656866000038 ) ) ;
#18771 = CARTESIAN_POINT ( 'NONE',  ( 15.03168679707239441, -3640.848700000039116, 2296.210799999999836 ) ) ;
#18772 = B_SPLINE_CURVE_WITH_KNOTS ( 'NONE', 3,
 ( #757, #6289, #9778, #15414, #18581, #13420, #20555, #4626, #2874, #7918, #22545, #18923, #10131, #20798, #4748, #11897, #2531, #16924, #19047, #2984, #9675, #658, #6866 ),
 .UNSPECIFIED., .F., .F.,
 ( 4, 2, 2, 1, 1, 2, 2, 2, 2, 1, 2, 2, 4 ),
 ( 0.000000000000000000, 0.1250000000062300443, 0.1875000000093439700, 0.2187500000104950215, 0.2343750000109342535, 0.2421875000111524123, 0.2500000000113705712, 0.3750000000063293260, 0.4375000000038087311, 0.4687500000027571279, 0.4843750000025556779, 0.5000000000023542279, 1.000000000000000000 ),
 .UNSPECIFIED. ) ;
#18773 = CARTESIAN_POINT ( 'NONE',  ( 12.69999999999999929, -3579.494999999999891, 2239.009999999999764 ) ) ;
#18774 = DATE_AND_TIME ( #4828, #8605 ) ;
#18775 = DIRECTION ( 'NONE',  ( -0.7249994335945011414, 0.000000000000000000, -0.6887494619146010688 ) ) ;
#18776 = ORIENTED_EDGE ( 'NONE', *, *, #8936, .T. ) ;
#18777 = CARTESIAN_POINT ( 'NONE',  ( 15.03168679714000078, -3598.151299999999992, 2292.781800000000203 ) ) ;
#18778 = AXIS2_PLACEMENT_3D ( 'NONE', #18101, #302, #21393 ) ;
#18779 = APPROVAL ( #243, 'UNSPECIFIED' ) ;
#18780 = CARTESIAN_POINT ( 'NONE',  ( -12.69999999999988027, -3578.860000000000127, 2252.472000000000207 ) ) ;
#18781 = LINE ( 'NONE', #20539, #8536 ) ;
#18782 = AXIS2_PLACEMENT_3D ( 'NONE', #9841, #8103, #15247 ) ;
#18783 = ORIENTED_EDGE ( 'NONE', *, *, #9138, .F. ) ;
#18784 = AXIS2_PLACEMENT_3D ( 'NONE', #5427, #1666, #8822 ) ;
#18785 = CARTESIAN_POINT ( 'NONE',  ( 136.9171347365734732, -3543.485052021662341, 2255.165528817252380 ) ) ;
#18786 = CIRCLE ( 'NONE', #16911, 11.11249999999999716 ) ;
#18787 = EDGE_CURVE ( 'NONE', #18259, #2462, #21993, .T. ) ;
#18788 = ORIENTED_EDGE ( 'NONE', *, *, #8594, .T. ) ;
#18789 = CARTESIAN_POINT ( 'NONE',  ( 142.5447999999989861, -3579.494999999999891, 2257.962944264955695 ) ) ;
#18790 = ADVANCED_FACE ( 'NONE', ( #15081 ), #1004, .T. ) ;
#18791 = CARTESIAN_POINT ( 'NONE',  ( 18.41519309054999454, -3659.279547307537541, 2244.670610241967097 ) ) ;
#18792 = ORIENTED_EDGE ( 'NONE', *, *, #5149, .F. ) ;
#18793 = EDGE_LOOP ( 'NONE', ( #11608, #17849, #2900, #1820, #18629 ) ) ;
#18794 = CARTESIAN_POINT ( 'NONE',  ( 72.59320000000001016, -3670.300000000000182, 2260.600000000000364 ) ) ;
#18795 = CARTESIAN_POINT ( 'NONE',  ( -8.890000000008999592, -3581.552400000000034, 2247.392000000000280 ) ) ;
#18796 = AXIS2_PLACEMENT_3D ( 'NONE', #2512, #8134, #6033 ) ;
#18797 = CARTESIAN_POINT ( 'NONE',  ( 12.69997737251000025, -3602.342301254000176, 2279.817638609000369 ) ) ;
#18798 = CARTESIAN_POINT ( 'NONE',  ( 101.5999999999999943, -3619.500000000000000, 2239.009999999999764 ) ) ;
#18799 = FACE_OUTER_BOUND ( 'NONE', #13212, .T. ) ;
#18800 = CARTESIAN_POINT ( 'NONE',  ( 136.8552000000009912, -3659.504999999999654, 2257.962944264955240 ) ) ;
#18801 = CIRCLE ( 'NONE', #6865, 3.606799999999001027 ) ;
#18802 = CARTESIAN_POINT ( 'NONE',  ( 116.8400000000000034, -3670.300000000000182, 2244.547199999999975 ) ) ;
#18803 = ORIENTED_EDGE ( 'NONE', *, *, #19838, .F. ) ;
#18804 = DATE_AND_TIME ( #15073, #21738 ) ;
#18805 = AXIS2_PLACEMENT_3D ( 'NONE', #19717, #11031, #14785 ) ;
#18806 = ORIENTED_EDGE ( 'NONE', *, *, #18279, .F. ) ;
#18807 = CARTESIAN_POINT ( 'NONE',  ( 145.3093031406643547, -3658.378945273449972, 2245.143073186572110 ) ) ;
#18808 = B_SPLINE_CURVE_WITH_KNOTS ( 'NONE', 3,
 ( #19408, #8975, #23025, #17522, #19636, #8865, #16008, #22905, #6998, #5469, #17993, #19765, #17639, #15778, #19522, #3694, #6880 ),
 .UNSPECIFIED., .F., .F.,
 ( 4, 2, 2, 1, 2, 2, 2, 2, 4 ),
 ( 0.000000000000000000, 0.1250000000007305545, 0.1875000000009396095, 0.2187500000009092449, 0.2343750000009681977, 0.2500000000010271228, 0.5000000000006847856, 0.7500000000003423928, 1.000000000000000000 ),
 .UNSPECIFIED. ) ;
#18809 = APPLIED_PERSON_AND_ORGANIZATION_ASSIGNMENT ( #2420, #2636, ( #16119 ) ) ;
#18810 = DIRECTION ( 'NONE',  ( 0.000000000000000000, -1.000000000000000000, 0.000000000000000000 ) ) ;
#18811 = DIRECTION ( 'NONE',  ( 0.000000000000000000, -1.000000000000000000, 0.000000000000000000 ) ) ;
#18812 = ORIENTED_EDGE ( 'NONE', *, *, #2065, .F. ) ;
#18813 = AXIS2_PLACEMENT_3D ( 'NONE', #19204, #1385, #908 ) ;
#18814 = CYLINDRICAL_SURFACE ( 'NONE', #5481, 2.844799999999999773 ) ;
#18815 = EDGE_CURVE ( 'NONE', #13878, #22201, #2886, .T. ) ;
#18816 = CARTESIAN_POINT ( 'NONE',  ( 144.7049814936195560, -3662.264031039746897, 2245.499284825724772 ) ) ;
#18817 = EDGE_LOOP ( 'NONE', ( #10701, #9749, #15639, #6000, #3384 ) ) ;
#18818 = AXIS2_PLACEMENT_3D ( 'NONE', #3448, #17743, #10366 ) ;
#18819 = CARTESIAN_POINT ( 'NONE',  ( 54.40679999999999694, -3568.700000000000273, 2239.771999999999935 ) ) ;
#18820 = ADVANCED_FACE ( 'NONE', ( #1117 ), #4645, .T. ) ;
#18821 = CARTESIAN_POINT ( 'NONE',  ( 14.40783068962525704, -3661.780600406073518, 2249.716311546600082 ) ) ;
#18822 = EDGE_CURVE ( 'NONE', #17874, #16212, #4183, .T. ) ;
#18823 = AXIS2_PLACEMENT_3D ( 'NONE', #17470, #20996, #1420 ) ;
#18824 = DIRECTION ( 'NONE',  ( -2.324635735433000053E-14, 2.336881798971000105E-14, -1.000000000000000000 ) ) ;
#18825 = ORIENTED_EDGE ( 'NONE', *, *, #9676, .F. ) ;
#18826 = CARTESIAN_POINT ( 'NONE',  ( 76.20000000000000284, -3568.700000000000273, 2239.009999999999764 ) ) ;
#18827 = CYLINDRICAL_SURFACE ( 'NONE', #12195, 0.7620000000000001217 ) ;
#18828 = CARTESIAN_POINT ( 'NONE',  ( 9.209369265603214672, -3695.699999999999818, 2282.113800000000083 ) ) ;
#18829 = DIRECTION ( 'NONE',  ( 1.000000000000000000, 0.000000000000000000, 0.000000000000000000 ) ) ;
#18830 = CARTESIAN_POINT ( 'NONE',  ( 12.69999999996000106, -3642.194899999999961, 2296.210799999999836 ) ) ;
#18831 = ORIENTED_EDGE ( 'NONE', *, *, #6378, .F. ) ;
#18832 = AXIS2_PLACEMENT_3D ( 'NONE', #19232, #3165, #19701 ) ;
#18833 = VERTEX_POINT ( 'NONE', #19175 ) ;
#18834 = VECTOR ( 'NONE', #9561, 1000.000000000000000 ) ;
#18835 = LINE ( 'NONE', #22457, #7212 ) ;
#18836 = EDGE_CURVE ( 'NONE', #9227, #8260, #1653, .T. ) ;
#18837 = VERTEX_POINT ( 'NONE', #8748 ) ;
#18838 = CARTESIAN_POINT ( 'NONE',  ( 9.652920519510999497, -3543.299999999999727, 2254.503999999999905 ) ) ;
#18839 = COORDINATED_UNIVERSAL_TIME_OFFSET ( 0, 0, .AHEAD. ) ;
#18840 = TOROIDAL_SURFACE ( 'NONE', #6886, 3.606799999998999695, 0.7620000000000000107 ) ;
#18841 = FACE_OUTER_BOUND ( 'NONE', #11050, .T. ) ;
#18842 = CYLINDRICAL_SURFACE ( 'NONE', #6017, 5.460999999999938126 ) ;
#18843 = CARTESIAN_POINT ( 'NONE',  ( 17.76256148820106873, -3662.156670368803134, 2245.385473685605120 ) ) ;
#18844 = CARTESIAN_POINT ( 'NONE',  ( 13.24918551347000140, -3656.709137200999521, 2257.605105471000115 ) ) ;
#18845 = DIRECTION ( 'NONE',  ( 0.000000000000000000, 0.000000000000000000, -1.000000000000000000 ) ) ;
#18846 = FACE_OUTER_BOUND ( 'NONE', #10610, .T. ) ;
#18847 = ORIENTED_EDGE ( 'NONE', *, *, #23017, .F. ) ;
#18848 = AXIS2_PLACEMENT_3D ( 'NONE', #7586, #11112, #18250 ) ;
#18849 = DIRECTION ( 'NONE',  ( 1.000000000000000000, 5.432398939370943590E-28, -2.324635735433000369E-14 ) ) ;
#18850 = EDGE_CURVE ( 'NONE', #15816, #159, #5044, .T. ) ;
#18851 = AXIS2_PLACEMENT_3D ( 'NONE', #11182, #18210, #3794 ) ;
#18852 = DIRECTION ( 'NONE',  ( 0.000000000000000000, -1.000000000000000000, 0.000000000000000000 ) ) ;
#18853 = ORIENTED_EDGE ( 'NONE', *, *, #5725, .T. ) ;
#18854 = LINE ( 'NONE', #13466, #11404 ) ;
#18855 = B_SPLINE_CURVE_WITH_KNOTS ( 'NONE', 3,
 ( #19489, #17724, #1672, #8829, #15977, #23109, #17960, #21714, #9299, #5787, #4128, #4020, #19961, #16549, #3665, #9056, #5669, #158, #16207, #1908, #20082, #7423, #21938, #10816, #9515, #7306, #11046, #386, #14687, #21608, #280, #19842, #2154, #12806, #16434, #21832, #14800, #12921, #5560, #9412, #14460, #12692, #22046, #16660, #11169, #3897, #3775, #18422, #14574, #16327, #18307, #10929, #5904, #11276, #18194, #2263, #7531, #502, #13041, #18079, #7640, #2029, #20190, #2379, #613, #9180, #7768, #14918, #6014, #13146, #17118, #4247, #11500, #11849, #8220, #8115, #10082, #1061 ),
 .UNSPECIFIED., .F., .F.,
 ( 4, 2, 2, 1, 2, 2, 2, 1, 2, 2, 2, 1, 2, 2, 2, 2, 2, 2, 1, 2, 2, 2, 2, 2, 1, 2, 2, 2, 2, 2, 2, 1, 2, 2, 2, 1, 2, 2, 2, 1, 2, 2, 4 ),
 ( 0.000000000000000000, 0.06249999999963576358, 0.09374999999935469674, 0.1093749999993084698, 0.1171874999992827404, 0.1249999999992570110, 0.1562499999990260291, 0.1718749999989712951, 0.1796874999989692134, 0.1874999999989671595, 0.2187499999990615007, 0.2343749999990822341, 0.2421874999990623334, 0.2499999999990424882, 0.2812499999990388244, 0.2968749999990641375, 0.3124999999990893951, 0.3437499999991340260, 0.3593749999991605604, 0.3671874999991988631, 0.3749999999992371658, 0.5000000000001054712, 0.5625000000005331291, 0.5937500000007637224, 0.6093750000008819612, 0.6171875000009465762, 0.6250000000010110801, 0.6562500000011579626, 0.6718750000012543300, 0.6875000000013506973, 0.7187500000014223067, 0.7343750000014820367, 0.7421875000015212276, 0.7500000000015604185, 0.7812500000013671286, 0.7968750000012251311, 0.8046875000011541879, 0.8125000000010832446, 0.8437500000008643086, 0.8593750000007152057, 0.8671875000006794565, 0.8750000000006435963, 1.000000000000000000 ),
 .UNSPECIFIED. ) ;
#18856 = CARTESIAN_POINT ( 'NONE',  ( 10.32556948557736831, -3657.938223185949937, 2249.193569921440940 ) ) ;
#18857 = EDGE_CURVE ( 'NONE', #12867, #17851, #18870, .T. ) ;
#18858 = VERTEX_POINT ( 'NONE', #15663 ) ;
#18859 = EDGE_CURVE ( 'NONE', #22597, #15845, #17364, .T. ) ;
#18860 = VERTEX_POINT ( 'NONE', #17398 ) ;
#18861 = PERSON_AND_ORGANIZATION_ROLE ( 'classification_officer' ) ;
#18862 = CARTESIAN_POINT ( 'NONE',  ( -12.54218463268301775, -3577.513799999511775, 2249.723686797000937 ) ) ;
#18863 = EDGE_LOOP ( 'NONE', ( #9351, #9643, #12909, #8897, #19820 ) ) ;
#18864 = DIRECTION ( 'NONE',  ( -1.000000000000000000, 0.000000000000000000, 0.000000000000000000 ) ) ;
#18865 = DIRECTION ( 'NONE',  ( 0.000000000000000000, 0.000000000000000000, 1.000000000000000000 ) ) ;
#18866 = CARTESIAN_POINT ( 'NONE',  ( 141.9451864939326526, -3581.242051290370000, 2248.947253967675806 ) ) ;
#18867 = EDGE_CURVE ( 'NONE', #16669, #14130, #14399, .T. ) ;
#18868 = ORIENTED_EDGE ( 'NONE', *, *, #2084, .T. ) ;
#18869 = CARTESIAN_POINT ( 'NONE',  ( 137.5573135925616555, -3661.385388595491349, 2257.800363168595140 ) ) ;
#18870 = CIRCLE ( 'NONE', #6921, 2.844800000000001550 ) ;
#18871 = SHAPE_DEFINITION_REPRESENTATION ( #1316, #13255 ) ;
#18872 = AXIS2_PLACEMENT_3D ( 'NONE', #8871, #12147, #3241 ) ;
#18873 = CARTESIAN_POINT ( 'NONE',  ( 61.26424768829000556, -3543.299999999999727, 2280.589800000000196 ) ) ;
#18874 = CARTESIAN_POINT ( 'NONE',  ( 20.57361267289067186, -3543.469596741131681, 2259.964971591370613 ) ) ;
#18875 = ADVANCED_FACE ( 'NONE', ( #21170 ), #21137, .T. ) ;
#18876 = CARTESIAN_POINT ( 'NONE',  ( 12.69999999999999929, -3659.504999999999654, 2239.771999999999935 ) ) ;
#18877 = EDGE_CURVE ( 'NONE', #13348, #15808, #22232, .T. ) ;
#18878 = ORIENTED_EDGE ( 'NONE', *, *, #17290, .T. ) ;
#18879 = CARTESIAN_POINT ( 'NONE',  ( 0.000000000000000000, -3694.430000000000291, 2240.279999999999745 ) ) ;
#18880 = VERTEX_POINT ( 'NONE', #6653 ) ;
#18881 = ORIENTED_EDGE ( 'NONE', *, *, #18084, .F. ) ;
#18882 = AXIS2_PLACEMENT_3D ( 'NONE', #21401, #3693, #19995 ) ;
#18883 = AXIS2_PLACEMENT_3D ( 'NONE', #7340, #419, #12953 ) ;
#18884 = EDGE_CURVE ( 'NONE', #17328, #3458, #22606, .T. ) ;
#18885 = DIRECTION ( 'NONE',  ( -1.000000000000000000, 0.000000000000000000, 0.000000000000000000 ) ) ;
#18886 = CIRCLE ( 'NONE', #19649, 2.844800000000091700 ) ;
#18887 = ORIENTED_EDGE ( 'NONE', *, *, #14046, .T. ) ;
#18888 = DIRECTION ( 'NONE',  ( 0.000000000000000000, 1.000000000000000000, 0.000000000000000000 ) ) ;
#18889 = DIRECTION ( 'NONE',  ( -1.000000000000000000, 0.000000000000000000, 0.000000000000000000 ) ) ;
#18890 = ORIENTED_EDGE ( 'NONE', *, *, #1403, .F. ) ;
#18891 = DIRECTION ( 'NONE',  ( 0.000000000000000000, -1.000000000000000000, 0.000000000000000000 ) ) ;
#18892 = DIRECTION ( 'NONE',  ( 0.000000000000000000, 1.000000000000000000, 0.000000000000000000 ) ) ;
#18893 = DIRECTION ( 'NONE',  ( -1.000000000000000000, 0.000000000000000000, 0.000000000000000000 ) ) ;
#18894 = PERSON_AND_ORGANIZATION ( #5446, #1895 ) ;
#18895 = DIRECTION ( 'NONE',  ( -1.000000000000000000, 0.000000000000000000, 0.000000000000000000 ) ) ;
#18896 = CARTESIAN_POINT ( 'NONE',  ( 12.69999999999999929, -3662.679999999999836, 2270.760000000000218 ) ) ;
#18897 = ORIENTED_EDGE ( 'NONE', *, *, #22504, .T. ) ;
#18898 = DIRECTION ( 'NONE',  ( 1.000000000000000000, 0.000000000000000000, 0.000000000000000000 ) ) ;
#18899 = AXIS2_PLACEMENT_3D ( 'NONE', #2497, #18885, #9416 ) ;
#18900 = CIRCLE ( 'NONE', #947, 3.606799999998994366 ) ;
#18901 = EDGE_CURVE ( 'NONE', #17031, #2645, #16622, .T. ) ;
#18902 = VECTOR ( 'NONE', #22476, 1000.000000000000000 ) ;
#18903 = CYLINDRICAL_SURFACE ( 'NONE', #14339, 1.269999999999882334 ) ;
#18904 = CYLINDRICAL_SURFACE ( 'NONE', #10397, 0.7620000000000000107 ) ;
#18905 = ORIENTED_EDGE ( 'NONE', *, *, #20842, .F. ) ;
#18906 = CARTESIAN_POINT ( 'NONE',  ( 88.90000000000000568, -3594.099999999999909, 2259.837999999999738 ) ) ;
#18907 = ORIENTED_EDGE ( 'NONE', *, *, #1830, .T. ) ;
#18908 = FACE_OUTER_BOUND ( 'NONE', #19793, .T. ) ;
#18909 = CARTESIAN_POINT ( 'NONE',  ( 18.26114034560631438, -3658.187853388129042, 2245.322692878756698 ) ) ;
#18910 = VERTEX_POINT ( 'NONE', #21051 ) ;
#18911 = ORIENTED_EDGE ( 'NONE', *, *, #15305, .F. ) ;
#18912 = DIRECTION ( 'NONE',  ( 0.000000000000000000, 1.000000000000000000, 0.000000000000000000 ) ) ;
#18913 = AXIS2_PLACEMENT_3D ( 'NONE', #4312, #15091, #13330 ) ;
#18914 = CARTESIAN_POINT ( 'NONE',  ( 20.09942059832000183, -3694.430000000000291, 2260.390449568000349 ) ) ;
#18915 = AXIS2_PLACEMENT_3D ( 'NONE', #16042, #17671, #8896 ) ;
#18916 = LINE ( 'NONE', #655, #15581 ) ;
#18917 = APPLIED_PERSON_AND_ORGANIZATION_ASSIGNMENT ( #1919, #22882, ( #20600 ) ) ;
#18918 = VERTEX_POINT ( 'NONE', #4998 ) ;
#18919 = CARTESIAN_POINT ( 'NONE',  ( 15.41268679701111566, -3637.936329547520472, 2296.591799999999694 ) ) ;
#18920 = AXIS2_PLACEMENT_3D ( 'NONE', #12751, #12639, #17908 ) ;
#18921 = DIRECTION ( 'NONE',  ( 0.000000000000000000, 0.000000000000000000, 1.000000000000000000 ) ) ;
#18922 = CARTESIAN_POINT ( 'NONE',  ( 137.4277151414249829, -3657.754018655572963, 2257.824198879471169 ) ) ;
#18923 = CARTESIAN_POINT ( 'NONE',  ( 20.63606354183824365, -3695.608900718220866, 2259.808339625531517 ) ) ;
#18924 = AXIS2_PLACEMENT_3D ( 'NONE', #6705, #19463, #12079 ) ;
#18925 = ORIENTED_EDGE ( 'NONE', *, *, #15516, .T. ) ;
#18926 = PERSON_AND_ORGANIZATION ( #5446, #1895 ) ;
#18927 = ORIENTED_EDGE ( 'NONE', *, *, #23023, .T. ) ;
#18928 = CIRCLE ( 'NONE', #10329, 4.114799999999974034 ) ;
#18929 = FACE_OUTER_BOUND ( 'NONE', #17499, .T. ) ;
#18930 = CARTESIAN_POINT ( 'NONE',  ( 9.956787186801534517, -3580.253871043101753, 2249.873812345001170 ) ) ;
#18931 = DIRECTION ( 'NONE',  ( 0.000000000000000000, 0.000000000000000000, -1.000000000000000000 ) ) ;
#18932 = AXIS2_PLACEMENT_3D ( 'NONE', #4972, #15759, #15873 ) ;
#18933 = ORIENTED_EDGE ( 'NONE', *, *, #7069, .F. ) ;
#18934 = CIRCLE ( 'NONE', #6978, 5.715000000000001634 ) ;
#18935 = CARTESIAN_POINT ( 'NONE',  ( 38.10000000000000142, -3644.899999999999636, 2260.600000000000364 ) ) ;
#18936 = TOROIDAL_SURFACE ( 'NONE', #8845, 5.588000000000000078, 0.7620000000000000107 ) ;
#18937 = DIRECTION ( 'NONE',  ( 0.000000000000000000, 0.000000000000000000, -1.000000000000000000 ) ) ;
#18938 = CARTESIAN_POINT ( 'NONE',  ( 145.3645409109730338, -3660.264428733753448, 2244.549527799832958 ) ) ;
#18939 = EDGE_LOOP ( 'NONE', ( #11111, #11615, #13870, #4914 ) ) ;
#18940 =( BOUNDED_CURVE ( )  B_SPLINE_CURVE ( 3, ( #3492, #16040, #23057, #10410 ),
 .UNSPECIFIED., .F., .T. ) 
 B_SPLINE_CURVE_WITH_KNOTS ( ( 4, 4 ),
 ( -9.769962616701377556E-15, 1.570796327117804925 ),
 .UNSPECIFIED. ) 
 CURVE ( )  GEOMETRIC_REPRESENTATION_ITEM ( )  RATIONAL_B_SPLINE_CURVE ( ( 1.000000000000000000, 0.8047378540482524878, 0.8047378540482524878, 1.000000000000000000 ) ) 
 REPRESENTATION_ITEM ( '' )  );
#18941 = CARTESIAN_POINT ( 'NONE',  ( 15.24000000000000021, -3578.213872745999652, 2255.774000000000342 ) ) ;
#18942 = CIRCLE ( 'NONE', #16326, 3.175000000000149925 ) ;
#18943 = CARTESIAN_POINT ( 'NONE',  ( 13.58859980245300925, -3662.207521219565933, 2249.346108138774980 ) ) ;
#18944 = CARTESIAN_POINT ( 'NONE',  ( -0.7620000000000000107, -3543.299999999999727, 2253.487999999999829 ) ) ;
#18945 = ORIENTED_EDGE ( 'NONE', *, *, #14986, .F. ) ;
#18946 = AXIS2_PLACEMENT_3D ( 'NONE', #20899, #17135, #19370 ) ;
#18947 = CARTESIAN_POINT ( 'NONE',  ( 63.50000000000000000, -3594.099999999999909, 2261.869999999999891 ) ) ;
#18948 = CARTESIAN_POINT ( 'NONE',  ( 15.48106175502000070, -3638.876388315999975, 2279.464089773000069 ) ) ;
#18949 = APPROVAL ( #11741, 'UNSPECIFIED' ) ;
#18950 = DIRECTION ( 'NONE',  ( 0.000000000000000000, 0.000000000000000000, -1.000000000000000000 ) ) ;
#18951 = CARTESIAN_POINT ( 'NONE',  ( 54.40679999999999694, -3619.500000000000000, 2239.009999999999764 ) ) ;
#18952 = DIRECTION ( 'NONE',  ( 0.000000000000000000, 0.000000000000000000, -1.000000000000000000 ) ) ;
#18953 = ORIENTED_EDGE ( 'NONE', *, *, #15467, .T. ) ;
#18954 = ORIENTED_EDGE ( 'NONE', *, *, #11274, .F. ) ;
#18955 = AXIS2_PLACEMENT_3D ( 'NONE', #2463, #16973, #11819 ) ;
#18956 = ADVANCED_FACE ( 'NONE', ( #4873 ), #17749, .T. ) ;
#18957 = ORIENTED_EDGE ( 'NONE', *, *, #19292, .F. ) ;
#18958 = CARTESIAN_POINT ( 'NONE',  ( 139.6999999999999886, -3577.590000000000146, 2270.760000000000218 ) ) ;
#18959 = EDGE_CURVE ( 'NONE', #3211, #13045, #2417, .T. ) ;
#18960 = EDGE_LOOP ( 'NONE', ( #3297, #13485, #2377 ) ) ;
#18961 = AXIS2_PLACEMENT_3D ( 'NONE', #3400, #1875, #2117 ) ;
#18962 = CARTESIAN_POINT ( 'NONE',  ( 9.850976268665682767, -3543.400907226547588, 2255.000110291591682 ) ) ;
#18963 = AXIS2_PLACEMENT_3D ( 'NONE', #1798, #13989, #22872 ) ;
#18964 = APPROVAL_DATE_TIME ( #22229, #176 ) ;
#18965 = ADVANCED_FACE ( 'NONE', ( #1469 ), #15777, .T. ) ;
#18966 = CARTESIAN_POINT ( 'NONE',  ( 116.8400000000000034, -3568.700000000000273, 2247.392000000000280 ) ) ;
#18967 = CARTESIAN_POINT ( 'NONE',  ( 34.49320000000000164, -3594.099999999999909, 2239.771999999999935 ) ) ;
#18968 = CARTESIAN_POINT ( 'NONE',  ( 61.26424768829000556, -3543.299999999999727, 2280.589800000000196 ) ) ;
#18969 = DIRECTION ( 'NONE',  ( 0.000000000000000000, 1.000000000000000000, 0.000000000000000000 ) ) ;
#18970 = CARTESIAN_POINT ( 'NONE',  ( 0.7620000000000000107, -3694.938000000000102, 2275.763800000000174 ) ) ;
#18971 = ADVANCED_FACE ( 'NONE', ( #6879 ), #21290, .T. ) ;
#18972 = CARTESIAN_POINT ( 'NONE',  ( 60.21459350832999746, -3543.299999999999727, 2280.170699136999701 ) ) ;
#18973 = ORIENTED_EDGE ( 'NONE', *, *, #7301, .F. ) ;
#18974 = VECTOR ( 'NONE', #18270, 1000.000000000000000 ) ;
#18975 = CARTESIAN_POINT ( 'NONE',  ( 12.69999999999999929, -3579.494999999999891, 2244.978999999999814 ) ) ;
#18976 = VECTOR ( 'NONE', #21624, 1000.000000000000000 ) ;
#18977 = PLANE ( 'NONE',  #12182 ) ;
#18978 = ORIENTED_EDGE ( 'NONE', *, *, #6586, .F. ) ;
#18979 = ADVANCED_FACE ( 'NONE', ( #1237 ), #14766, .T. ) ;
#18980 = CARTESIAN_POINT ( 'NONE',  ( -12.31900000000000084, -3662.489255679000053, 2246.035656601000028 ) ) ;
#18981 = CARTESIAN_POINT ( 'NONE',  ( 10.54044424447347872, -3657.652706350100743, 2248.773822481034131 ) ) ;
#18982 = EDGE_CURVE ( 'NONE', #18582, #13004, #22989, .T. ) ;
#18983 = EDGE_LOOP ( 'NONE', ( #5093, #165 ) ) ;
#18984 = ORIENTED_EDGE ( 'NONE', *, *, #7303, .F. ) ;
#18985 = CARTESIAN_POINT ( 'NONE',  ( 134.2831716143903691, -3581.316932381290826, 2245.957881525630000 ) ) ;
#18986 = ORIENTED_EDGE ( 'NONE', *, *, #8557, .T. ) ;
#18987 = LINE ( 'NONE', #13597, #296 ) ;
#18988 = DIRECTION ( 'NONE',  ( 0.000000000000000000, 0.000000000000000000, -1.000000000000000000 ) ) ;
#18989 = DIRECTION ( 'NONE',  ( 1.000000000000000000, 0.000000000000000000, 0.000000000000000000 ) ) ;
#18990 = CARTESIAN_POINT ( 'NONE',  ( 142.3276510892873148, -3580.585198262936956, 2249.654023945091012 ) ) ;
#18991 = VERTEX_POINT ( 'NONE', #15541 ) ;
#18992 = DIRECTION ( 'NONE',  ( 0.000000000000000000, 0.000000000000000000, 1.000000000000000000 ) ) ;
#18993 = COORDINATED_UNIVERSAL_TIME_OFFSET ( 0, 0, .AHEAD. ) ;
#18994 = EDGE_CURVE ( 'NONE', #16380, #9946, #10269, .T. ) ;
#18995 = AXIS2_PLACEMENT_3D ( 'NONE', #13033, #18525, #20622 ) ;
#18996 = DIRECTION ( 'NONE',  ( 0.000000000000000000, 0.000000000000000000, -1.000000000000000000 ) ) ;
#18997 = CARTESIAN_POINT ( 'NONE',  ( 14.69151175564311451, -3581.526608352788571, 2248.384429562235255 ) ) ;
#18998 = EDGE_CURVE ( 'NONE', #6114, #21855, #21634, .T. ) ;
#18999 = CIRCLE ( 'NONE', #21986, 0.7619999999999294005 ) ;
#19000 = FACE_OUTER_BOUND ( 'NONE', #4342, .T. ) ;
#19001 = AXIS2_PLACEMENT_3D ( 'NONE', #11599, #2144, #11160 ) ;
#19002 = EDGE_LOOP ( 'NONE', ( #14010, #14425, #12826, #2796 ) ) ;
#19003 = DIRECTION ( 'NONE',  ( 1.000000000000000000, 0.000000000000000000, 0.000000000000000000 ) ) ;
#19004 = CYLINDRICAL_SURFACE ( 'NONE', #6556, 0.7619999999999294005 ) ;
#19005 = ORIENTED_EDGE ( 'NONE', *, *, #16300, .F. ) ;
#19006 = DIRECTION ( 'NONE',  ( 0.000000000000000000, 0.000000000000000000, -1.000000000000000000 ) ) ;
#19007 = CIRCLE ( 'NONE', #8529, 3.606800000000021100 ) ;
#19008 = ORIENTED_EDGE ( 'NONE', *, *, #20859, .T. ) ;
#19009 = CARTESIAN_POINT ( 'NONE',  ( 139.6999999999999886, -3668.712499999999636, 2268.705139999999574 ) ) ;
#19010 = CARTESIAN_POINT ( 'NONE',  ( 25.39999999999999858, -3578.860000000000127, 2247.392000000000280 ) ) ;
#19011 = ORIENTED_EDGE ( 'NONE', *, *, #13410, .F. ) ;
#19012 = CIRCLE ( 'NONE', #3287, 1.269999999999882334 ) ;
#19013 = DIRECTION ( 'NONE',  ( 0.000000000000000000, 0.000000000000000000, 1.000000000000000000 ) ) ;
#19014 = DIRECTION ( 'NONE',  ( 0.000000000000000000, 0.000000000000000000, -1.000000000000000000 ) ) ;
#19015 =( LENGTH_UNIT ( ) NAMED_UNIT ( * ) SI_UNIT ( .MILLI., .METRE. ) );
#19016 = CARTESIAN_POINT ( 'NONE',  ( 139.6999999999999886, -3659.504999999999654, 2244.978999999999814 ) ) ;
#19017 = DIRECTION ( 'NONE',  ( 0.000000000000000000, 1.000000000000000000, 0.000000000000000000 ) ) ;
#19018 = CALENDAR_DATE ( 2026, 26, 10 ) ;
#19019 = CARTESIAN_POINT ( 'NONE',  ( 17.78000000000000114, -3659.504999999999654, 2239.391000000000076 ) ) ;
#19020 = CARTESIAN_POINT ( 'NONE',  ( -5.588000000000000078, -3578.860000000000127, 2247.392000000000280 ) ) ;
#19021 = CARTESIAN_POINT ( 'NONE',  ( 63.50000000000000000, -3644.899999999999636, 2260.600000000000364 ) ) ;
#19022 = EDGE_CURVE ( 'NONE', #15102, #6114, #12887, .T. ) ;
#19023 = CARTESIAN_POINT ( 'NONE',  ( 141.4940465161450902, -3657.297238990916867, 2247.526929148741146 ) ) ;
#19024 = EDGE_CURVE ( 'NONE', #22154, #17967, #20743, .T. ) ;
#19025 = DIRECTION ( 'NONE',  ( -1.000000000000000000, 0.000000000000000000, 0.000000000000000000 ) ) ;
#19026 = EDGE_CURVE ( 'NONE', #1205, #17905, #415, .T. ) ;
#19027 = EDGE_LOOP ( 'NONE', ( #7040, #6666, #8164 ) ) ;
#19028 = CARTESIAN_POINT ( 'NONE',  ( 137.1570006975785816, -3544.409801988883373, 2255.766426251236680 ) ) ;
#19029 = EDGE_CURVE ( 'NONE', #650, #5595, #541, .T. ) ;
#19030 = ORIENTED_EDGE ( 'NONE', *, *, #7294, .T. ) ;
#19031 = CARTESIAN_POINT ( 'NONE',  ( 4.618254035022729020, -3695.699999999998909, 2259.443539527655957 ) ) ;
#19032 = CARTESIAN_POINT ( 'NONE',  ( 12.69999999999999929, -3659.504999999999654, 2272.030000000000200 ) ) ;
#19033 = ORIENTED_EDGE ( 'NONE', *, *, #19816, .T. ) ;
#19034 = ORIENTED_EDGE ( 'NONE', *, *, #13450, .T. ) ;
#19035 = DIRECTION ( 'NONE',  ( -1.000000000000000000, 0.000000000000000000, 0.000000000000000000 ) ) ;
#19036 = DIRECTION ( 'NONE',  ( -1.000000000000000000, 0.000000000000000000, 0.000000000000000000 ) ) ;
#19037 = LINE ( 'NONE', #13527, #17440 ) ;
#19038 = ADVANCED_FACE ( 'NONE', ( #14717 ), #2182, .T. ) ;
#19039 = ORIENTED_EDGE ( 'NONE', *, *, #14395, .F. ) ;
#19040 = DIRECTION ( 'NONE',  ( 1.000000000000000000, 0.000000000000000000, 0.000000000000000000 ) ) ;
#19041 = ADVANCED_FACE ( 'NONE', ( #19764 ), #6940, .T. ) ;
#19042 = CARTESIAN_POINT ( 'NONE',  ( 15.03168679706412902, -3638.156299999897783, 2296.210799999999836 ) ) ;
#19043 = CARTESIAN_POINT ( 'NONE',  ( 55.57575231171000496, -3543.299999999999727, 2275.763800000000174 ) ) ;
#19044 = B_SPLINE_CURVE_WITH_KNOTS ( 'NONE', 3,
 ( #22543, #6515, #11764, #6747, #13890, #13777, #21036, #5304, #12447, #18922, #20797, #19045, #4506, #11644, #11896, #18800 ),
 .UNSPECIFIED., .F., .F.,
 ( 4, 2, 2, 2, 2, 2, 2, 4 ),
 ( 0.004462701392653794369, 0.005020548996892072041, 0.005578396601130348846, 0.006136244205368626518, 0.006694091809606903323, 0.007809787018084332968, 0.008367634622322985341, 0.008925482226561637714 ),
 .UNSPECIFIED. ) ;
#19045 = CARTESIAN_POINT ( 'NONE',  ( 137.0026594722382072, -3658.582242386909456, 2257.924723982745491 ) ) ;
#19046 = AXIS2_PLACEMENT_3D ( 'NONE', #6313, #13441, #20581 ) ;
#19047 = CARTESIAN_POINT ( 'NONE',  ( 20.52513111806586465, -3695.450320587698570, 2260.086246565152578 ) ) ;
#19048 = EDGE_LOOP ( 'NONE', ( #19912, #16541, #14506, #5749 ) ) ;
#19049 = DATE_AND_TIME ( #11899, #4515 ) ;
#19050 = VERTEX_POINT ( 'NONE', #7450 ) ;
#19051 = CYLINDRICAL_SURFACE ( 'NONE', #18014, 5.460999999999938126 ) ;
#19052 = CARTESIAN_POINT ( 'NONE',  ( 10.31734595597029625, -3581.049170776430856, 2249.208705551349340 ) ) ;
#19053 = CARTESIAN_POINT ( 'NONE',  ( -0.7620000000000000107, -3543.299999999999727, 2239.771999999999935 ) ) ;
#19054 = ORIENTED_EDGE ( 'NONE', *, *, #898, .F. ) ;
#19055 = DIRECTION ( 'NONE',  ( 0.000000000000000000, 0.000000000000000000, -1.000000000000000000 ) ) ;
#19056 = CIRCLE ( 'NONE', #14944, 3.606799999999993567 ) ;
#19057 = DIRECTION ( 'NONE',  ( 1.000000000000000000, 0.000000000000000000, 0.000000000000000000 ) ) ;
#19058 = CARTESIAN_POINT ( 'NONE',  ( 144.4943168350663143, -3662.615994720476920, 2245.990590281715413 ) ) ;
#19059 = VECTOR ( 'NONE', #21644, 1000.000000000000000 ) ;
#19060 = DIRECTION ( 'NONE',  ( 0.000000000000000000, 0.000000000000000000, -1.000000000000000000 ) ) ;
#19061 = DIRECTION ( 'NONE',  ( 0.000000000000000000, 0.000000000000000000, -1.000000000000000000 ) ) ;
#19062 = CARTESIAN_POINT ( 'NONE',  ( 147.3506172137967098, -3544.133557168236621, 2260.523297438373447 ) ) ;
#19063 = EDGE_LOOP ( 'NONE', ( #15606, #10841 ) ) ;
#19064 = CARTESIAN_POINT ( 'NONE',  ( 14.21033367406000103, -3637.084566859999995, 2279.715678855999613 ) ) ;
#19065 = DIRECTION ( 'NONE',  ( 2.347365683444999541E-13, 0.000000000000000000, -1.000000000000000000 ) ) ;
#19066 = DIRECTION ( 'NONE',  ( 0.5000000000031612490, -0.8660254037826135010, 0.000000000000000000 ) ) ;
#19067 = CYLINDRICAL_SURFACE ( 'NONE', #5341, 2.844799999999999773 ) ;
#19068 = VERTEX_POINT ( 'NONE', #4046 ) ;
#19069 = ORIENTED_EDGE ( 'NONE', *, *, #1841, .F. ) ;
#19070 = AXIS2_PLACEMENT_3D ( 'NONE', #9262, #16400, #11347 ) ;
#19071 = DIRECTION ( 'NONE',  ( 0.000000000000000000, 0.000000000000000000, -1.000000000000000000 ) ) ;
#19072 = LOCAL_TIME ( 17, 37, 43.00000000000000000, #15498 ) ;
#19073 = EDGE_LOOP ( 'NONE', ( #19818, #10294, #10790, #17832 ) ) ;
#19074 = CIRCLE ( 'NONE', #20550, 2.844799999999052531 ) ;
#19075 = CARTESIAN_POINT ( 'NONE',  ( 12.69998522105638905, -3636.657698770827210, 2279.817639764999967 ) ) ;
#19076 = APPROVAL_DATE_TIME ( #8415, #10617 ) ;
#19077 = CARTESIAN_POINT ( 'NONE',  ( 12.69999999994000106, -3596.805100000000039, 2296.210799999999836 ) ) ;
#19078 = DIRECTION ( 'NONE',  ( 6.341789985291834412E-14, 0.000000000000000000, 1.000000000000000000 ) ) ;
#19079 = CARTESIAN_POINT ( 'NONE',  ( 12.69999999999999929, -3579.494999999999891, 2239.391000000000076 ) ) ;
#19080 =( BOUNDED_CURVE ( )  B_SPLINE_CURVE ( 3, ( #10372, #22552, #22669, #13658 ),
 .UNSPECIFIED., .F., .T. ) 
 B_SPLINE_CURVE_WITH_KNOTS ( ( 4, 4 ),
 ( 1.570796326625032657, 3.141592653589783346 ),
 .UNSPECIFIED. ) 
 CURVE ( )  GEOMETRIC_REPRESENTATION_ITEM ( )  RATIONAL_B_SPLINE_CURVE ( ( 1.000000000000000000, 0.8047378540843299621, 0.8047378540843299621, 1.000000000000000000 ) ) 
 REPRESENTATION_ITEM ( '' )  );
#19081 = DIRECTION ( 'NONE',  ( -6.475491540587999912E-14, 2.590196616235000036E-13, -1.000000000000000000 ) ) ;
#19082 = APPLIED_PERSON_AND_ORGANIZATION_ASSIGNMENT ( #1518, #3394, ( #5262 ) ) ;
#19083 = DIRECTION ( 'NONE',  ( 0.000000000000000000, 0.000000000000000000, -1.000000000000000000 ) ) ;
#19084 = DIRECTION ( 'NONE',  ( -1.000000000000000000, 2.330758767201999921E-14, 2.343004830739999973E-14 ) ) ;
#19085 = VERTEX_POINT ( 'NONE', #14602 ) ;
#19086 = CARTESIAN_POINT ( 'NONE',  ( -6.731000000000127770, -3660.140000000000327, 2241.931000000000040 ) ) ;
#19087 = ADVANCED_FACE ( 'NONE', ( #9327 ), #20039, .T. ) ;
#19088 = DIRECTION ( 'NONE',  ( 0.000000000000000000, 0.000000000000000000, -1.000000000000000000 ) ) ;
#19089 = ORIENTED_EDGE ( 'NONE', *, *, #133, .T. ) ;
#19090 = APPLIED_APPROVAL_ASSIGNMENT ( #14222, ( #19460 ) ) ;
#19091 = ADVANCED_FACE ( 'NONE', ( #16237 ), #11191, .F. ) ;
#19092 = DIRECTION ( 'NONE',  ( 1.000000000000000000, -3.885294924347999634E-13, 0.000000000000000000 ) ) ;
#19093 = CARTESIAN_POINT ( 'NONE',  ( 10.05440704136412222, -3658.459147675929671, 2249.687161261317669 ) ) ;
#19094 = EDGE_CURVE ( 'NONE', #15095, #4452, #19278, .T. ) ;
#19095 = VERTEX_POINT ( 'NONE', #187 ) ;
#19096 = ORIENTED_EDGE ( 'NONE', *, *, #13572, .T. ) ;
#19097 = CARTESIAN_POINT ( 'NONE',  ( 133.9977473889447879, -3579.940010871619506, 2244.748233079255897 ) ) ;
#19098 = ORIENTED_EDGE ( 'NONE', *, *, #11232, .F. ) ;
#19099 = PRODUCT ( 'Screw 1', 'Screw 1', '', ( #2842 ) ) ;
#19100 = LINE ( 'NONE', #15470, #21569 ) ;
#19101 = DIRECTION ( 'NONE',  ( 0.000000000000000000, 0.000000000000000000, 1.000000000000000000 ) ) ;
#19102 = EDGE_CURVE ( 'NONE', #23061, #12468, #10872, .T. ) ;
#19103 = CARTESIAN_POINT ( 'NONE',  ( -12.69999999999999929, -3661.706170452999686, 2250.104686796999886 ) ) ;
#19104 = ORIENTED_EDGE ( 'NONE', *, *, #18156, .T. ) ;
#19105 = CARTESIAN_POINT ( 'NONE',  ( -12.69999999999999929, -3581.992340905000219, 2247.392000000000280 ) ) ;
#19106 = APPLICATION_PROTOCOL_DEFINITION ( 'international standard', 'automotive_design', 2000, #7699 ) ;
#19107 = DIRECTION ( 'NONE',  ( 0.7249994335945011414, 0.000000000000000000, 0.6887494619146010688 ) ) ;
#19108 = B_SPLINE_CURVE_WITH_KNOTS ( 'NONE', 3,
 ( #6802, #13943, #5036, #3386, #12181, #10537 ),
 .UNSPECIFIED., .F., .F.,
 ( 4, 1, 1, 4 ),
 ( 0.000000000000000000, 0.3333333333333000081, 0.6666666666667000474, 1.000000000000000000 ),
 .UNSPECIFIED. ) ;
#19109 = APPROVAL_PERSON_ORGANIZATION ( #22460, #10617, #13810 ) ;
#19110 = CARTESIAN_POINT ( 'NONE',  ( 14.74624570788535394, -3581.471973361198252, 2248.523728683949685 ) ) ;
#19111 = APPROVAL_PERSON_ORGANIZATION ( #12218, #7921, #150 ) ;
#19112 = CARTESIAN_POINT ( 'NONE',  ( 38.10000000000000142, -3644.899999999999636, 2239.771999999999935 ) ) ;
#19113 = ORIENTED_EDGE ( 'NONE', *, *, #22759, .T. ) ;
#19114 = CARTESIAN_POINT ( 'NONE',  ( 15.59751622981730534, -3695.643849727398901, 2254.879165046700564 ) ) ;
#19115 = EDGE_CURVE ( 'NONE', #4467, #14916, #9907, .T. ) ;
#19116 = CARTESIAN_POINT ( 'NONE',  ( 12.70000000005999929, -3576.802599999999984, 2242.820000000000164 ) ) ;
#19117 = ORIENTED_EDGE ( 'NONE', *, *, #19810, .F. ) ;
#19118 = DIRECTION ( 'NONE',  ( -1.000000000000000000, 0.000000000000000000, 0.000000000000000000 ) ) ;
#19119 = EDGE_CURVE ( 'NONE', #11590, #20602, #17992, .T. ) ;
#19120 = EDGE_CURVE ( 'NONE', #14878, #2758, #7337, .T. ) ;
#19121 = DIRECTION ( 'NONE',  ( 0.000000000000000000, 0.000000000000000000, -1.000000000000000000 ) ) ;
#19122 = ORIENTED_EDGE ( 'NONE', *, *, #13239, .T. ) ;
#19123 = ORIENTED_EDGE ( 'NONE', *, *, #9392, .T. ) ;
#19124 = APPLIED_SECURITY_CLASSIFICATION_ASSIGNMENT ( #19492, ( #23172 ) ) ;
#19125 = CARTESIAN_POINT ( 'NONE',  ( 133.9849999999999852, -3659.504999999999654, 2239.771999999999935 ) ) ;
#19126 = APPLIED_APPROVAL_ASSIGNMENT ( #18949, ( #10138 ) ) ;
#19127 = ORIENTED_EDGE ( 'NONE', *, *, #4149, .F. ) ;
#19128 = FACE_BOUND ( 'NONE', #3672, .T. ) ;
#19129 = DIRECTION ( 'NONE',  ( 0.000000000000000000, 0.000000000000000000, -1.000000000000000000 ) ) ;
#19130 =( NAMED_UNIT ( * ) PLANE_ANGLE_UNIT ( ) SI_UNIT ( $, .RADIAN. ) );
#19131 = CARTESIAN_POINT ( 'NONE',  ( 15.11851036462000053, -3601.006922181999926, 2279.551735152999754 ) ) ;
#19132 = PERSON ( 'NAUO-PER4', 'UNSPECIFIED', 'UNSPECIFIED', ('UNSPECIFIED'), ('UNSPECIFIED'), ('UNSPECIFIED') ) ;
#19134 = FACE_OUTER_BOUND ( 'NONE', #8763, .T. ) ;
#19133 = AXIS2_PLACEMENT_3D ( 'NONE', #7812, #14854, #5950 ) ;
#19135 = APPROVAL_ROLE ( '' ) ;
#19136 = VECTOR ( 'NONE', #18912, 1000.000000000000000 ) ;
#19137 = CARTESIAN_POINT ( 'NONE',  ( 151.4000000000000057, -3578.860000000000127, 2250.265832635400784 ) ) ;
#19138 = CARTESIAN_POINT ( 'NONE',  ( 15.41268679713999923, -3601.063670452999759, 2296.591799999999694 ) ) ;
#19139 = CARTESIAN_POINT ( 'NONE',  ( 19.05000000000000071, -3578.860000000000127, 2247.392000000000280 ) ) ;
#19140 = EDGE_CURVE ( 'NONE', #11962, #22306, #12489, .T. ) ;
#19141 = CARTESIAN_POINT ( 'NONE',  ( 141.6348846241527895, -3657.419409829039068, 2248.223748579871426 ) ) ;
#19142 = ORIENTED_EDGE ( 'NONE', *, *, #10667, .F. ) ;
#19143 = CARTESIAN_POINT ( 'NONE',  ( 136.8057571348549288, -3543.355825686663138, 2254.886068102028275 ) ) ;
#19144 = VERTEX_POINT ( 'NONE', #17880 ) ;
#19145 = CIRCLE ( 'NONE', #11299, 0.7619999999999294005 ) ;
#19146 = CARTESIAN_POINT ( 'NONE',  ( 22.55520000000100111, -3670.300000000000182, 2259.837999999999738 ) ) ;
#19147 = AXIS2_PLACEMENT_3D ( 'NONE', #12209, #3178, #22973 ) ;
#19148 = DIRECTION ( 'NONE',  ( -1.000000000000000000, 0.000000000000000000, 0.000000000000000000 ) ) ;
#19149 = ORIENTED_EDGE ( 'NONE', *, *, #21483, .T. ) ;
#19150 = ORIENTED_EDGE ( 'NONE', *, *, #7283, .F. ) ;
#19151 = CARTESIAN_POINT ( 'NONE',  ( 15.03168679710911704, -3660.851200000110111, 2239.391000000000076 ) ) ;
#19152 = DIRECTION ( 'NONE',  ( 0.000000000000000000, 0.000000000000000000, -1.000000000000000000 ) ) ;
#19153 = CARTESIAN_POINT ( 'NONE',  ( 72.59320000000001016, -3568.700000000000273, 2260.600000000000364 ) ) ;
#19154 = EDGE_CURVE ( 'NONE', #16084, #5789, #10907, .T. ) ;
#19155 = EDGE_LOOP ( 'NONE', ( #6573, #17964, #11481, #10823, #17468 ) ) ;
#19156 = EDGE_CURVE ( 'NONE', #18481, #4457, #15160, .T. ) ;
#19157 = DIRECTION ( 'NONE',  ( 1.000000000000000000, 0.000000000000000000, 0.000000000000000000 ) ) ;
#19158 = DIRECTION ( 'NONE',  ( -1.000000000000000000, 0.000000000000000000, 0.000000000000000000 ) ) ;
#19159 = DIRECTION ( 'NONE',  ( 0.000000000000000000, -1.000000000000000000, 0.000000000000000000 ) ) ;
#19160 = DIRECTION ( 'NONE',  ( 1.000000000000000000, 0.000000000000000000, 0.000000000000000000 ) ) ;
#19161 = LINE ( 'NONE', #3217, #19246 ) ;
#19162 = EDGE_LOOP ( 'NONE', ( #10091, #12088, #17303, #14948 ) ) ;
#19163 = APPROVAL_ROLE ( '' ) ;
#19164 = ORIENTED_EDGE ( 'NONE', *, *, #21025, .T. ) ;
#19165 = LINE ( 'NONE', #17630, #8665 ) ;
#19166 = VECTOR ( 'NONE', #4201, 1000.000000000000000 ) ;
#19167 = ADVANCED_FACE ( 'NONE', ( #22073 ), #19004, .T. ) ;
#19168 = CIRCLE ( 'NONE', #800, 0.7619999999999294005 ) ;
#19169 = CARTESIAN_POINT ( 'NONE',  ( 0.000000000000000000, -3660.140000000000327, 2247.392000000000280 ) ) ;
#19170 = CARTESIAN_POINT ( 'NONE',  ( 50.79999999999999716, -3619.500000000000000, 2261.869999999999891 ) ) ;
#19171 = ORIENTED_EDGE ( 'NONE', *, *, #3988, .T. ) ;
#19172 = EDGE_CURVE ( 'NONE', #3301, #10484, #5433, .T. ) ;
#19173 = FACE_OUTER_BOUND ( 'NONE', #12010, .T. ) ;
#19174 = EDGE_CURVE ( 'NONE', #22087, #8066, #3056, .T. ) ;
#19175 = CARTESIAN_POINT ( 'NONE',  ( 22.54063073453000143, -3544.061999999999898, 2275.001800000000003 ) ) ;
#19176 = CARTESIAN_POINT ( 'NONE',  ( 144.6754166191346940, -3662.317343768547744, 2245.560154884797612 ) ) ;
#19177 = DIRECTION ( 'NONE',  ( 2.336881798971000105E-14, 0.000000000000000000, 1.000000000000000000 ) ) ;
#19178 = AXIS2_PLACEMENT_3D ( 'NONE', #17986, #17872, #9089 ) ;
#19179 = CARTESIAN_POINT ( 'NONE',  ( 11.19369693972251412, -3661.918311847638961, 2249.612478909842594 ) ) ;
#19180 = CARTESIAN_POINT ( 'NONE',  ( 139.6999999999999886, -3662.197400000000016, 2239.391000000000076 ) ) ;
#19181 = VERTEX_POINT ( 'NONE', #10204 ) ;
#19182 = CIRCLE ( 'NONE', #99, 2.844799999999994444 ) ;
#19183 = CARTESIAN_POINT ( 'NONE',  ( 47.95519999999999783, -3670.300000000000182, 2259.837999999999738 ) ) ;
#19184 = AXIS2_PLACEMENT_3D ( 'NONE', #11425, #755, #17625 ) ;
#19185 = DIRECTION ( 'NONE',  ( 0.000000000000000000, 0.000000000000000000, -1.000000000000000000 ) ) ;
#19186 = AXIS2_PLACEMENT_3D ( 'NONE', #21894, #20255, #6315 ) ;
#19187 = ADVANCED_FACE ( 'NONE', ( #1295 ), #6039, .T. ) ;
#19188 = CARTESIAN_POINT ( 'NONE',  ( 63.50000000000000000, -3644.899999999999636, 2239.771999999999935 ) ) ;
#19189 = CARTESIAN_POINT ( 'NONE',  ( 15.39205606714550711, -3658.584397266909491, 2249.774343474533453 ) ) ;
#19190 = LINE ( 'NONE', #17534, #4575 ) ;
#19191 = EDGE_LOOP ( 'NONE', ( #5958, #20885, #3053, #10125 ) ) ;
#19192 = VERTEX_POINT ( 'NONE', #22739 ) ;
#19193 = ORIENTED_EDGE ( 'NONE', *, *, #468, .F. ) ;
#19194 = CARTESIAN_POINT ( 'NONE',  ( 12.79204376678999999, -3582.339799989999847, 2257.592639999999847 ) ) ;
#19196 = AXIS2_PLACEMENT_3D ( 'NONE', #15256, #3049, #13484 ) ;
#19195 = ITEM_DEFINED_TRANSFORMATION ( 'NONE', 'NONE', #7125,  #5611 ) ;
#19197 = DIRECTION ( 'NONE',  ( 0.000000000000000000, 0.000000000000000000, -1.000000000000000000 ) ) ;
#19198 = ORIENTED_EDGE ( 'NONE', *, *, #12299, .T. ) ;
#19199 = CARTESIAN_POINT ( 'NONE',  ( 142.4535506740546964, -3578.756509080423257, 2257.939127564392948 ) ) ;
#19200 = CARTESIAN_POINT ( 'NONE',  ( 12.70000000005999929, -3656.812599999999748, 2242.820000000000164 ) ) ;
#19201 = B_SPLINE_CURVE_WITH_KNOTS ( 'NONE', 3,
 ( #20714, #11811, #2909, #19199, #15333, #1140, #3138, #20595, #903, #22350, #4436, #20488, #1381, #8544, #22230, #8072 ),
 .UNSPECIFIED., .F., .F.,
 ( 4, 2, 2, 2, 2, 2, 2, 4 ),
 ( 0.004462717107651111709, 0.005020574082334379636, 0.005578431057017647562, 0.006136288031700915489, 0.006694145006384183416, 0.007809858955751593571, 0.008367715930435238800, 0.008925572905118884029 ),
 .UNSPECIFIED. ) ;
#19202 = AXIS2_PLACEMENT_3D ( 'NONE', #7916, #2872, #18684 ) ;
#19203 = CARTESIAN_POINT ( 'NONE',  ( 15.21772229205999949, -3658.170722075999947, 2257.881333375999930 ) ) ;
#19204 = CARTESIAN_POINT ( 'NONE',  ( 35.56000000000000227, -3544.570000000000164, 2247.392000000000280 ) ) ;
#19205 = AXIS2_PLACEMENT_3D ( 'NONE', #14560, #11151, #16194 ) ;
#19206 = FACE_OUTER_BOUND ( 'NONE', #13149, .T. ) ;
#19207 = ORIENTED_EDGE ( 'NONE', *, *, #21182, .F. ) ;
#19208 = FACE_OUTER_BOUND ( 'NONE', #4524, .T. ) ;
#19209 = CYLINDRICAL_SURFACE ( 'NONE', #8443, 0.3809999999999121312 ) ;
#19210 = EDGE_LOOP ( 'NONE', ( #701, #16865, #11887, #8669 ) ) ;
#19211 = CARTESIAN_POINT ( 'NONE',  ( -12.31900000000000084, -3657.447599999999966, 2247.392000000000280 ) ) ;
#19212 = CARTESIAN_POINT ( 'NONE',  ( 10.73839315088192592, -3657.443723703987416, 2248.304826634740948 ) ) ;
#19213 = CIRCLE ( 'NONE', #13958, 0.7619999999999987894 ) ;
#19214 = ORIENTED_EDGE ( 'NONE', *, *, #9872, .F. ) ;
#19215 = ORIENTED_EDGE ( 'NONE', *, *, #17685, .T. ) ;
#19216 = CARTESIAN_POINT ( 'NONE',  ( 134.1499366578294428, -3580.855533714581725, 2245.364243621502283 ) ) ;
#19217 = AXIS2_PLACEMENT_3D ( 'NONE', #2170, #18321, #295 ) ;
#19218 = ORIENTED_EDGE ( 'NONE', *, *, #22168, .F. ) ;
#19219 = APPLIED_DATE_AND_TIME_ASSIGNMENT ( #7242, #12631, ( #19492 ) ) ;
#19220 = VECTOR ( 'NONE', #16664, 1000.000000000000114 ) ;
#19221 = CARTESIAN_POINT ( 'NONE',  ( 20.82707948048999924, -3543.299999999999727, 2259.329999999999927 ) ) ;
#19222 = DATE_AND_TIME ( #19338, #12756 ) ;
#19223 = CARTESIAN_POINT ( 'NONE',  ( 15.24000000000000021, -3580.776127254000130, 2255.774000000000342 ) ) ;
#19224 = EDGE_LOOP ( 'NONE', ( #4188, #12420, #5125, #19553 ) ) ;
#19225 = CARTESIAN_POINT ( 'NONE',  ( 132.0583097651000060, -3694.797466901999996, 2260.545675974999995 ) ) ;
#19226 = PERSON_AND_ORGANIZATION ( #5446, #1895 ) ;
#19227 = EDGE_CURVE ( 'NONE', #22764, #3735, #14833, .T. ) ;
#19228 = CARTESIAN_POINT ( 'NONE',  ( -0.2667862122801000213, -3694.430000000000291, 2239.290827591999914 ) ) ;
#19229 = CARTESIAN_POINT ( 'NONE',  ( 15.21492942528371373, -3580.825415784637698, 2249.449528553973778 ) ) ;
#19230 = AXIS2_PLACEMENT_3D ( 'NONE', #4545, #2790, #17082 ) ;
#19231 = CARTESIAN_POINT ( 'NONE',  ( 134.0541150472915888, -3658.613793347861701, 2244.987821917966812 ) ) ;
#19232 = CARTESIAN_POINT ( 'NONE',  ( -0.7620000000000000107, -3660.140000000000327, 2247.392000000000280 ) ) ;
#19233 = ORIENTED_EDGE ( 'NONE', *, *, #9137, .T. ) ;
#19234 = CARTESIAN_POINT ( 'NONE',  ( 15.55240168165168058, -3695.602652332858270, 2254.991658124059086 ) ) ;
#19235 = CARTESIAN_POINT ( 'NONE',  ( 13.78135004281000064, -3576.858789906999846, 2257.644359223000265 ) ) ;
#19236 = ORIENTED_EDGE ( 'NONE', *, *, #16718, .F. ) ;
#19237 = FACE_OUTER_BOUND ( 'NONE', #15925, .T. ) ;
#19238 = CARTESIAN_POINT ( 'NONE',  ( 35.56000000000000227, -3694.430000000000291, 2247.392000000000280 ) ) ;
#19239 = EDGE_LOOP ( 'NONE', ( #2521, #4449, #11333, #4536 ) ) ;
#19240 = ORIENTED_EDGE ( 'NONE', *, *, #3776, .T. ) ;
#19241 = CYLINDRICAL_SURFACE ( 'NONE', #2311, 2.844799999998995244 ) ;
#19242 = CARTESIAN_POINT ( 'NONE',  ( 134.0191424391260568, -3660.128805427137195, 2244.547198930071318 ) ) ;
#19243 = VECTOR ( 'NONE', #21108, 1000.000000000000000 ) ;
#19244 = ORIENTED_EDGE ( 'NONE', *, *, #281, .F. ) ;
#19245 = PRODUCT_RELATED_PRODUCT_CATEGORY ( 'detail', '', ( #16320 ) ) ;
#19246 = VECTOR ( 'NONE', #517, 1000.000000000000000 ) ;
#19247 = FACE_OUTER_BOUND ( 'NONE', #12260, .T. ) ;
#19248 = CARTESIAN_POINT ( 'NONE',  ( 136.6539306146721913, -3657.399154367426945, 2246.629994581112896 ) ) ;
#19249 = CARTESIAN_POINT ( 'NONE',  ( 59.89320000000000022, -3644.899999999999636, 2239.771999999999935 ) ) ;
#19250 = AXIS2_PLACEMENT_3D ( 'NONE', #22568, #9801, #6537 ) ;
#19251 = CARTESIAN_POINT ( 'NONE',  ( 20.32000000000000028, -3578.860000000000127, 2247.392000000000280 ) ) ;
#19252 = APPROVAL_DATE_TIME ( #6373, #22502 ) ;
#19253 = ADVANCED_FACE ( 'NONE', ( #17341 ), #18517, .T. ) ;
#19254 = CARTESIAN_POINT ( 'NONE',  ( 35.56000000000000227, -3670.300000000000182, 2244.547199999999975 ) ) ;
#19255 = CARTESIAN_POINT ( 'NONE',  ( 12.69999999999999929, -3599.497499999999945, 2264.841800000000148 ) ) ;
#19257 = EDGE_CURVE ( 'NONE', #3416, #17982, #13735, .T. ) ;
#19256 = DIRECTION ( 'NONE',  ( 0.000000000000000000, 0.000000000000000000, -1.000000000000000000 ) ) ;
#19258 = EDGE_CURVE ( 'NONE', #11298, #10072, #2516, .T. ) ;
#19259 = CARTESIAN_POINT ( 'NONE',  ( 142.0244369740106833, -3657.864944588135131, 2249.100147049036877 ) ) ;
#19260 = ORIENTED_EDGE ( 'NONE', *, *, #2969, .T. ) ;
#19261 = VECTOR ( 'NONE', #22209, 1000.000000000000114 ) ;
#19262 = CARTESIAN_POINT ( 'NONE',  ( 139.6999999999999886, -3659.504999999999654, 2245.359999999999673 ) ) ;
#19263 = AXIS2_PLACEMENT_3D ( 'NONE', #16239, #8978, #74 ) ;
#19264 = ORIENTED_EDGE ( 'NONE', *, *, #3055, .T. ) ;
#19265 = TOROIDAL_SURFACE ( 'NONE', #14403, 4.114799999999999791, 1.270000000000000018 ) ;
#19266 = VERTEX_POINT ( 'NONE', #11301 ) ;
#19267 = CARTESIAN_POINT ( 'NONE',  ( 61.26424768829000556, -3695.699999999999818, 2279.065800000000309 ) ) ;
#19268 = VERTEX_POINT ( 'NONE', #15611 ) ;
#19269 = EDGE_LOOP ( 'NONE', ( #17672, #14404 ) ) ;
#19270 = CARTESIAN_POINT ( 'NONE',  ( 8.986184632732999944, -3694.938000000000102, 2281.890615367000009 ) ) ;
#19271 = EDGE_CURVE ( 'NONE', #17496, #19453, #4934, .T. ) ;
#19272 = LINE ( 'NONE', #19389, #12151 ) ;
#19273 = DIRECTION ( 'NONE',  ( 0.000000000000000000, -1.000000000000000000, 0.000000000000000000 ) ) ;
#19274 = EDGE_LOOP ( 'NONE', ( #22871, #18890, #19743, #2674 ) ) ;
#19275 = CARTESIAN_POINT ( 'NONE',  ( 15.41268679701173738, -3597.931329547518999, 2296.591799999999694 ) ) ;
#19276 = DIRECTION ( 'NONE',  ( 1.000000000000000000, 0.000000000000000000, 0.000000000000000000 ) ) ;
#19277 = VECTOR ( 'NONE', #5674, 999.9999999999998863 ) ;
#19278 = CIRCLE ( 'NONE', #2786, 2.844799999999994444 ) ;
#19279 = LINE ( 'NONE', #5222, #13705 ) ;
#19280 = EDGE_LOOP ( 'NONE', ( #18812, #9393, #6110, #2558 ) ) ;
#19281 = APPROVAL_DATE_TIME ( #12125, #18237 ) ;
#19282 = AXIS2_PLACEMENT_3D ( 'NONE', #6332, #13707, #2681 ) ;
#19283 = ORIENTED_EDGE ( 'NONE', *, *, #14820, .F. ) ;
#19284 = CIRCLE ( 'NONE', #13674, 5.715000000000997282 ) ;
#19285 = DIRECTION ( 'NONE',  ( 0.000000000000000000, 0.000000000000000000, 1.000000000000000000 ) ) ;
#19286 = EDGE_CURVE ( 'NONE', #16839, #923, #20879, .T. ) ;
#19287 = CARTESIAN_POINT ( 'NONE',  ( 10.87999328488129969, -3581.681618670022090, 2247.764026984493739 ) ) ;
#19288 = SPHERICAL_SURFACE ( 'NONE', #14582, 0.7620000000000000107 ) ;
#19289 = ORIENTED_EDGE ( 'NONE', *, *, #3814, .T. ) ;
#19290 = FACE_BOUND ( 'NONE', #8918, .T. ) ;
#19291 = ADVANCED_FACE ( 'NONE', ( #20331 ), #10085, .T. ) ;
#19292 = EDGE_CURVE ( 'NONE', #2120, #1044, #4273, .T. ) ;
#19293 = CIRCLE ( 'NONE', #13295, 0.7619999999999294005 ) ;
#19294 = DIRECTION ( 'NONE',  ( 0.000000000000000000, 0.000000000000000000, -1.000000000000000000 ) ) ;
#19295 = CARTESIAN_POINT ( 'NONE',  ( 144.8951781795001068, -3661.886301090974939, 2245.146221596522082 ) ) ;
#19296 = LINE ( 'NONE', #21292, #2494 ) ;
#19297 = CIRCLE ( 'NONE', #11788, 0.3809999999999647002 ) ;
#19298 = CARTESIAN_POINT ( 'NONE',  ( 20.32000000000000028, -3670.300000000000182, 2289.213099999999940 ) ) ;
#19299 = PRODUCT_DEFINITION_SHAPE ( 'NONE', 'NONE',  #22639 ) ;
#19300 = CARTESIAN_POINT ( 'NONE',  ( 147.3828687998903035, -3543.951823051294468, 2260.442383242537289 ) ) ;
#19301 = AXIS2_PLACEMENT_3D ( 'NONE', #6072, #7938, #20473 ) ;
#19302 = ORIENTED_EDGE ( 'NONE', *, *, #8781, .T. ) ;
#19303 = CARTESIAN_POINT ( 'NONE',  ( 142.2400000000000091, -3580.776127254000130, 2255.774000000000342 ) ) ;
#19304 = CYLINDRICAL_SURFACE ( 'NONE', #13313, 0.7619999999999294005 ) ;
#19305 = DIRECTION ( 'NONE',  ( 0.000000000000000000, 0.000000000000000000, -1.000000000000000000 ) ) ;
#19306 = CARTESIAN_POINT ( 'NONE',  ( 15.07032488946356352, -3657.931869745440963, 2249.185847854341773 ) ) ;
#19307 = DIRECTION ( 'NONE',  ( 1.000000000000000000, 0.000000000000000000, -1.224646799147353207E-16 ) ) ;
#19308 = ORIENTED_EDGE ( 'NONE', *, *, #3188, .T. ) ;
#19309 = ADVANCED_FACE ( 'NONE', ( #18564 ), #17230, .T. ) ;
#19310 = ORIENTED_EDGE ( 'NONE', *, *, #2924, .F. ) ;
#19311 = FACE_OUTER_BOUND ( 'NONE', #12546, .T. ) ;
#19312 = VECTOR ( 'NONE', #21464, 1000.000000000000000 ) ;
#19313 = EDGE_LOOP ( 'NONE', ( #17965, #22388, #15930, #12188 ) ) ;
#19314 = CARTESIAN_POINT ( 'NONE',  ( 10.36831320283000046, -3640.848700000000008, 2292.781800000000203 ) ) ;
#19315 = AXIS2_PLACEMENT_3D ( 'NONE', #14150, #17404, #15548 ) ;
#19316 = DATE_AND_TIME ( #7127, #18367 ) ;
#19317 = CARTESIAN_POINT ( 'NONE',  ( 12.69999999999999929, -3659.504999999999654, 2246.630000000000109 ) ) ;
#19318 = CIRCLE ( 'NONE', #17424, 3.606799999999993567 ) ;
#19319 = CARTESIAN_POINT ( 'NONE',  ( 142.0316867971391162, -3578.148799999964467, 2239.391000000000076 ) ) ;
#19320 = DIRECTION ( 'NONE',  ( 0.000000000000000000, -1.000000000000000000, 0.000000000000000000 ) ) ;
#19321 = AXIS2_PLACEMENT_3D ( 'NONE', #21515, #7104, #19634 ) ;
#19322 = CARTESIAN_POINT ( 'NONE',  ( 139.6999999999999886, -3659.504999999999654, 2272.030000000000200 ) ) ;
#19323 = CARTESIAN_POINT ( 'NONE',  ( 19.05000000000000071, -3660.140000000000327, 2247.392000000000280 ) ) ;
#19324 = ADVANCED_FACE ( 'NONE', ( #6153 ), #13286, .T. ) ;
#19325 = DIRECTION ( 'NONE',  ( 0.000000000000000000, -1.000000000000000000, 0.000000000000000000 ) ) ;
#19326 = ORIENTED_EDGE ( 'NONE', *, *, #15595, .T. ) ;
#19327 = CARTESIAN_POINT ( 'NONE',  ( 12.69999999996000106, -3642.194899999999961, 2292.781800000000203 ) ) ;
#19328 = VERTEX_POINT ( 'NONE', #22616 ) ;
#19329 = CARTESIAN_POINT ( 'NONE',  ( -6.349999999999999645, -3656.965000000000146, 2247.392000000000280 ) ) ;
#19330 = CARTESIAN_POINT ( 'NONE',  ( 10.19155798493820697, -3658.160642684393679, 2249.438182561015310 ) ) ;
#19331 = AXIS2_PLACEMENT_3D ( 'NONE', #12819, #23123, #5329 ) ;
#19332 = ORIENTED_EDGE ( 'NONE', *, *, #9433, .T. ) ;
#19333 = CARTESIAN_POINT ( 'NONE',  ( 12.69999999999999929, -3589.528000000000247, 2275.055139999999483 ) ) ;
#19334 = ADVANCED_FACE ( 'NONE', ( #21344 ), #7305, .T. ) ;
#19335 = EDGE_CURVE ( 'NONE', #2445, #9572, #7276, .T. ) ;
#19336 = VERTEX_POINT ( 'NONE', #5180 ) ;
#19337 = CARTESIAN_POINT ( 'NONE',  ( 12.69999999999999929, -3579.494999999999891, 2239.771999999999935 ) ) ;
#19338 = CALENDAR_DATE ( 2026, 26, 10 ) ;
#19339 = CARTESIAN_POINT ( 'NONE',  ( 130.6067999999989979, -3568.700000000000273, 2239.771999999999935 ) ) ;
#19340 = ORIENTED_EDGE ( 'NONE', *, *, #14104, .T. ) ;
#19341 = FACE_OUTER_BOUND ( 'NONE', #16760, .T. ) ;
#19342 = DATE_AND_TIME ( #6922, #13481 ) ;
#19343 = CARTESIAN_POINT ( 'NONE',  ( 7.020348529275000082, -3578.860230781999689, 2244.548186305999934 ) ) ;
#19344 = DIRECTION ( 'NONE',  ( 0.000000000000000000, 0.000000000000000000, 1.000000000000000000 ) ) ;
#19345 = AXIS2_PLACEMENT_3D ( 'NONE', #14338, #36, #21482 ) ;
#19346 = CARTESIAN_POINT ( 'NONE',  ( 134.2542439495752262, -3657.771239293389954, 2245.816275623240472 ) ) ;
#19347 = VECTOR ( 'NONE', #845, 1000.000000000000000 ) ;
#19348 = CARTESIAN_POINT ( 'NONE',  ( 127.0000000000000000, -3568.700000000000273, 2239.771999999999935 ) ) ;
#19349 = ORIENTED_EDGE ( 'NONE', *, *, #4140, .T. ) ;
#19350 = AXIS2_PLACEMENT_3D ( 'NONE', #9485, #695, #14993 ) ;
#19351 = CARTESIAN_POINT ( 'NONE',  ( 0.7620000000000000107, -3544.061999999999898, 2295.829799999999977 ) ) ;
#19352 = CARTESIAN_POINT ( 'NONE',  ( 14.03517516284999900, -3576.977758144000290, 2257.672197071000028 ) ) ;
#19353 = ORIENTED_EDGE ( 'NONE', *, *, #15293, .F. ) ;
#19354 = CARTESIAN_POINT ( 'NONE',  ( 57.14999999999999858, -3694.430000000000291, 2247.392000000000280 ) ) ;
#19355 = DIRECTION ( 'NONE',  ( -0.000000000000000000, 1.000000000000000000, 0.000000000000000000 ) ) ;
#19356 = ORIENTED_EDGE ( 'NONE', *, *, #21535, .F. ) ;
#19357 = ORIENTED_EDGE ( 'NONE', *, *, #4726, .T. ) ;
#19358 = DIRECTION ( 'NONE',  ( 1.000000000000000000, 0.000000000000000000, 0.000000000000000000 ) ) ;
#19359 = DIRECTION ( 'NONE',  ( 0.000000000000000000, 0.000000000000000000, 1.000000000000000000 ) ) ;
#19360 =( BOUNDED_CURVE ( )  B_SPLINE_CURVE ( 3, ( #17041, #1104, #22424, #13653 ),
 .UNSPECIFIED., .F., .F. ) 
 B_SPLINE_CURVE_WITH_KNOTS ( ( 4, 4 ),
 ( -2.664535259100375697E-14, 1.570796326280532895 ),
 .UNSPECIFIED. ) 
 CURVE ( )  GEOMETRIC_REPRESENTATION_ITEM ( )  RATIONAL_B_SPLINE_CURVE ( ( 1.000000000000000000, 0.8047378542455954076, 0.8047378542455954076, 1.000000000000000000 ) ) 
 REPRESENTATION_ITEM ( '' )  );
#19361 = ORIENTED_EDGE ( 'NONE', *, *, #21943, .F. ) ;
#19362 = AXIS2_PLACEMENT_3D ( 'NONE', #21594, #5423, #10918 ) ;
#19363 = DIRECTION ( 'NONE',  ( -1.000000000000000000, 0.000000000000000000, 0.000000000000000000 ) ) ;
#19364 = DIRECTION ( 'NONE',  ( 0.8660254037817868289, -0.5000000000045929927, -1.484475890920977686E-12 ) ) ;
#19365 = CARTESIAN_POINT ( 'NONE',  ( 15.54478274857000031, -3659.509919104000346, 2250.166342301999521 ) ) ;
#19366 = CYLINDRICAL_SURFACE ( 'NONE', #626, 2.844799999999999773 ) ;
#19367 = APPROVAL_DATE_TIME ( #16312, #3045 ) ;
#19368 = CIRCLE ( 'NONE', #5533, 3.606799999999993567 ) ;
#19369 = AXIS2_PLACEMENT_3D ( 'NONE', #8568, #10197, #3046 ) ;
#19370 = DIRECTION ( 'NONE',  ( 0.000000000000000000, 0.000000000000000000, 1.000000000000000000 ) ) ;
#19371 = CARTESIAN_POINT ( 'NONE',  ( 12.69999999999999929, -3644.963499999999840, 2296.210799999999836 ) ) ;
#19372 = CARTESIAN_POINT ( 'NONE',  ( 18.37347785155967728, -3580.182493284099110, 2244.873281192540617 ) ) ;
#19373 = CARTESIAN_POINT ( 'NONE',  ( 141.5058393440477005, -3657.306719107069966, 2247.135511502391637 ) ) ;
#19374 = EDGE_LOOP ( 'NONE', ( #3319, #5438, #19929, #19164 ) ) ;
#19375 = DIRECTION ( 'NONE',  ( 0.000000000000000000, -1.000000000000000000, 0.000000000000000000 ) ) ;
#19376 = APPLIED_PERSON_AND_ORGANIZATION_ASSIGNMENT ( #7208, #10722, ( #12017 ) ) ;
#19377 = AXIS2_PLACEMENT_3D ( 'NONE', #16256, #14275, #3365 ) ;
#19378 = EDGE_LOOP ( 'NONE', ( #16629, #10876 ) ) ;
#19379 = ORIENTED_EDGE ( 'NONE', *, *, #8158, .F. ) ;
#19380 = ORIENTED_EDGE ( 'NONE', *, *, #6161, .F. ) ;
#19381 = AXIS2_PLACEMENT_3D ( 'NONE', #10665, #22958, #21573 ) ;
#19382 = DIRECTION ( 'NONE',  ( 0.000000000000000000, 0.000000000000000000, -1.000000000000000000 ) ) ;
#19383 = EDGE_CURVE ( 'NONE', #21039, #22822, #21113, .T. ) ;
#19384 = ORIENTED_EDGE ( 'NONE', *, *, #18736, .F. ) ;
#19385 = ORIENTED_EDGE ( 'NONE', *, *, #11813, .F. ) ;
#19386 = CARTESIAN_POINT ( 'NONE',  ( 4.771292762646392127, -3543.401189131885076, 2259.826759462805512 ) ) ;
#19387 = EDGE_CURVE ( 'NONE', #9415, #10881, #10323, .T. ) ;
#19388 = COORDINATED_UNIVERSAL_TIME_OFFSET ( 0, 0, .AHEAD. ) ;
#19389 = CARTESIAN_POINT ( 'NONE',  ( 15.54479999999999862, -3579.494999999999891, 2272.030000000000200 ) ) ;
#19390 = CARTESIAN_POINT ( 'NONE',  ( 47.19319999999999737, -3619.500000000000000, 2259.837999999999738 ) ) ;
#19391 = ADVANCED_FACE ( 'NONE', ( #15721 ), #10287, .T. ) ;
#19392 = ORIENTED_EDGE ( 'NONE', *, *, #706, .T. ) ;
#19393 = CARTESIAN_POINT ( 'NONE',  ( 136.8551999999999964, -3579.494999999999891, 2256.063560000000052 ) ) ;
#19394 = CARTESIAN_POINT ( 'NONE',  ( 10.16000000000000014, -3580.776127254000130, 2255.774000000000342 ) ) ;
#19395 = DIRECTION ( 'NONE',  ( 0.000000000000000000, 1.000000000000000000, 0.000000000000000000 ) ) ;
#19396 = CARTESIAN_POINT ( 'NONE',  ( 17.78000000000000114, -3599.497499999999945, 2296.210799999999836 ) ) ;
#19397 = EDGE_LOOP ( 'NONE', ( #6697, #18011, #6215, #5984, #4931, #19233, #10993, #21144 ) ) ;
#19398 = APPROVAL_STATUS ( 'not_yet_approved' ) ;
#19399 = ORIENTED_EDGE ( 'NONE', *, *, #6803, .F. ) ;
#19400 = ADVANCED_FACE ( 'NONE', ( #16 ), #10671, .T. ) ;
#19401 = DIRECTION ( 'NONE',  ( 0.000000000000000000, -1.000000000000000000, 0.000000000000000000 ) ) ;
#19402 = CARTESIAN_POINT ( 'NONE',  ( 25.39999999999999858, -3619.500000000000000, 2259.837999999999738 ) ) ;
#19403 = DIRECTION ( 'NONE',  ( -1.000000000000000000, 0.000000000000000000, 0.000000000000000000 ) ) ;
#19404 = EDGE_CURVE ( 'NONE', #10059, #14578, #16181, .T. ) ;
#19405 = VERTEX_POINT ( 'NONE', #7165 ) ;
#19406 = DIRECTION ( 'NONE',  ( 0.000000000000000000, 1.000000000000000000, 0.000000000000000000 ) ) ;
#19407 = DIRECTION ( 'NONE',  ( 0.000000000000000000, 1.000000000000000000, 0.000000000000000000 ) ) ;
#19408 = CARTESIAN_POINT ( 'NONE',  ( 144.3113860273000171, -3576.119152860999748, 2246.630000000000109 ) ) ;
#19409 = DIRECTION ( 'NONE',  ( 0.000000000000000000, 0.000000000000000000, 1.000000000000000000 ) ) ;
#19410 = CARTESIAN_POINT ( 'NONE',  ( 11.26131265196617193, -3661.959416329594205, 2249.579061434116738 ) ) ;
#19411 = ORIENTED_EDGE ( 'NONE', *, *, #4541, .F. ) ;
#19412 = CARTESIAN_POINT ( 'NONE',  ( 142.0316867971961869, -3658.158799999862822, 2239.167815367171897 ) ) ;
#19413 = ORIENTED_EDGE ( 'NONE', *, *, #10239, .T. ) ;
#19414 = CARTESIAN_POINT ( 'NONE',  ( 142.4431999999993366, -3580.373257047432162, 2255.967040000000907 ) ) ;
#19415 = AXIS2_PLACEMENT_3D ( 'NONE', #3498, #21555, #339 ) ;
#19416 = ADVANCED_FACE ( 'NONE', ( #14315 ), #18151, .T. ) ;
#19417 = DIRECTION ( 'NONE',  ( 0.8660254037827048723, 0.5000000000030029312, 0.000000000000000000 ) ) ;
#19418 = EDGE_CURVE ( 'NONE', #698, #12971, #19539, .T. ) ;
#19419 = CARTESIAN_POINT ( 'NONE',  ( 12.69999999996000106, -3602.189899999999852, 2292.781800000000203 ) ) ;
#19420 = CARTESIAN_POINT ( 'NONE',  ( 15.33695353576711007, -3658.437581818261151, 2249.671216759049457 ) ) ;
#19421 = FACE_OUTER_BOUND ( 'NONE', #8744, .T. ) ;
#19422 = EDGE_LOOP ( 'NONE', ( #3262, #11187, #5673, #10349 ) ) ;
#19423 = CARTESIAN_POINT ( 'NONE',  ( 10.27280990245528258, -3578.011077221096457, 2250.107236679559264 ) ) ;
#19424 = ORIENTED_EDGE ( 'NONE', *, *, #11518, .T. ) ;
#19425 = CARTESIAN_POINT ( 'NONE',  ( 88.90000000000000568, -3594.099999999999909, 2259.837999999999738 ) ) ;
#19426 = ADVANCED_BREP_SHAPE_REPRESENTATION ( '', ( #13515, #5611 ), #1485 ) ;
#19427 = CYLINDRICAL_SURFACE ( 'NONE', #10778, 2.844799999999994444 ) ;
#19428 = APPROVAL_DATE_TIME ( #17421, #20631 ) ;
#19429 = DIRECTION ( 'NONE',  ( 1.000000000000000000, 0.000000000000000000, 0.000000000000000000 ) ) ;
#19430 = CARTESIAN_POINT ( 'NONE',  ( 10.06337286646999907, -3658.424665316000301, 2257.909780569999839 ) ) ;
#19431 = CARTESIAN_POINT ( 'NONE',  ( 10.68478392833999990, -3661.519597158000124, 2257.776259854999807 ) ) ;
#19432 = EDGE_CURVE ( 'NONE', #13851, #2102, #4564, .T. ) ;
#19433 = AXIS2_PLACEMENT_3D ( 'NONE', #19884, #21528, #7460 ) ;
#19434 = DIRECTION ( 'NONE',  ( 0.000000000000000000, 0.000000000000000000, -1.000000000000000000 ) ) ;
#19435 = CARTESIAN_POINT ( 'NONE',  ( 17.51847272801180466, -3576.421590885849128, 2245.925646346420308 ) ) ;
#19436 = DIRECTION ( 'NONE',  ( 2.330758767208999958E-14, 1.000000000000000000, 2.848874176402999842E-12 ) ) ;
#19437 = ORIENTED_EDGE ( 'NONE', *, *, #14540, .T. ) ;
#19438 = CARTESIAN_POINT ( 'NONE',  ( 12.69999999999999929, -3570.287499999999909, 2268.705139999999574 ) ) ;
#19439 = CARTESIAN_POINT ( 'NONE',  ( 6.222999999999998977, -3579.494999999999891, 2239.771999999999935 ) ) ;
#19440 = ORIENTED_EDGE ( 'NONE', *, *, #7879, .T. ) ;
#19441 = DIRECTION ( 'NONE',  ( -1.000000000000000000, 0.000000000000000000, 0.000000000000000000 ) ) ;
#19442 = EDGE_LOOP ( 'NONE', ( #10829, #1351 ) ) ;
#19443 = CARTESIAN_POINT ( 'NONE',  ( 134.1618273608623610, -3580.901497745790493, 2245.410526384101104 ) ) ;
#19444 = ORIENTED_EDGE ( 'NONE', *, *, #742, .F. ) ;
#19445 = AXIS2_PLACEMENT_3D ( 'NONE', #12709, #21503, #19747 ) ;
#19446 = VERTEX_POINT ( 'NONE', #13961 ) ;
#19447 = ORIENTED_EDGE ( 'NONE', *, *, #17163, .T. ) ;
#19448 = DIRECTION ( 'NONE',  ( -2.324635735433000053E-14, 2.336881798971000105E-14, -1.000000000000000000 ) ) ;
#19449 = ADVANCED_FACE ( 'NONE', ( #15835 ), #22620, .T. ) ;
#19450 = APPROVAL_STATUS ( 'not_yet_approved' ) ;
#19451 = EDGE_CURVE ( 'NONE', #10440, #22481, #15919, .T. ) ;
#19452 = DIRECTION ( 'NONE',  ( 0.000000000000000000, 1.000000000000000000, 0.000000000000000000 ) ) ;
#19453 = VERTEX_POINT ( 'NONE', #5880 ) ;
#19454 = CARTESIAN_POINT ( 'NONE',  ( 101.5999999999999943, -3619.500000000000000, 2239.009999999999764 ) ) ;
#19455 = PERSON_AND_ORGANIZATION ( #5446, #1895 ) ;
#19456 = CARTESIAN_POINT ( 'NONE',  ( 142.4126867972053674, -3661.071170452545175, 2239.009999999999764 ) ) ;
#19457 = CARTESIAN_POINT ( 'NONE',  ( 12.69999999999999929, -3648.710000000000036, 2268.705139999999574 ) ) ;
#19458 = CYLINDRICAL_SURFACE ( 'NONE', #18961, 0.3809999999998115450 ) ;
#19459 = CARTESIAN_POINT ( 'NONE',  ( -8.890000000017000303, -3577.513800000000174, 2249.723686796999573 ) ) ;
#19460 = SECURITY_CLASSIFICATION ( '', '', #1548 ) ;
#19461 = CARTESIAN_POINT ( 'NONE',  ( 3.810000000000000053, -3694.938000000000102, 2238.248000000000047 ) ) ;
#19462 = ORIENTED_EDGE ( 'NONE', *, *, #7379, .F. ) ;
#19463 = DIRECTION ( 'NONE',  ( -1.000000000000000000, 0.000000000000000000, 0.000000000000000000 ) ) ;
#19464 = EDGE_CURVE ( 'NONE', #830, #20690, #13122, .T. ) ;
#19465 = EDGE_CURVE ( 'NONE', #12928, #1840, #11765, .T. ) ;
#19466 = CARTESIAN_POINT ( 'NONE',  ( 13.51849986531999903, -3576.765770756000165, 2257.621751478000078 ) ) ;
#19467 = ORIENTED_EDGE ( 'NONE', *, *, #22303, .F. ) ;
#19468 = CARTESIAN_POINT ( 'NONE',  ( 88.90000000000000568, -3594.099999999999909, 2239.771999999999935 ) ) ;
#19469 = CARTESIAN_POINT ( 'NONE',  ( 20.09942059832000183, -3544.570000000000164, 2260.390449568000349 ) ) ;
#19470 = EDGE_LOOP ( 'NONE', ( #11692, #20241, #9400, #11262, #14721 ) ) ;
#19471 = DIRECTION ( 'NONE',  ( 0.000000000000000000, 0.000000000000000000, -1.000000000000000000 ) ) ;
#19472 = FACE_BOUND ( 'NONE', #12056, .T. ) ;
#19473 = AXIS2_PLACEMENT_3D ( 'NONE', #12512, #17901, #12287 ) ;
#19474 = ORIENTED_EDGE ( 'NONE', *, *, #1795, .F. ) ;
#19475 = CARTESIAN_POINT ( 'NONE',  ( 9.956800000000452400, -3658.626742952519635, 2255.967039999999997 ) ) ;
#19476 = EDGE_CURVE ( 'NONE', #15258, #22364, #1671, .T. ) ;
#19477 = DIRECTION ( 'NONE',  ( 1.000000000000000000, 0.000000000000000000, 0.000000000000000000 ) ) ;
#19478 = SHAPE_REPRESENTATION_RELATIONSHIP ( 'NONE' , 'NONE' ,  #16547, #2374 ) ;
#19479 = APPLIED_SECURITY_CLASSIFICATION_ASSIGNMENT ( #28, ( #10864 ) ) ;
#19480 = APPLIED_APPROVAL_ASSIGNMENT ( #15092, ( #22959 ) ) ;
#19481 = DIRECTION ( 'NONE',  ( 0.000000000000000000, 0.000000000000000000, 1.000000000000000000 ) ) ;
#19482 = APPROVAL_STATUS ( 'not_yet_approved' ) ;
#19483 = AXIS2_PLACEMENT_3D ( 'NONE', #5303, #7176, #14330 ) ;
#19484 = CARTESIAN_POINT ( 'NONE',  ( 134.0204252830999962, -3660.140268639000169, 2244.547525601999951 ) ) ;
#19485 = DIRECTION ( 'NONE',  ( 0.000000000000000000, 0.000000000000000000, -1.000000000000000000 ) ) ;
#19486 = DIRECTION ( 'NONE',  ( -1.224646799147353207E-16, 1.000000000000000000, 0.000000000000000000 ) ) ;
#19487 = CARTESIAN_POINT ( 'NONE',  ( 137.9049381359793358, -3657.298025595380295, 2247.542742861386614 ) ) ;
#19488 = ORIENTED_EDGE ( 'NONE', *, *, #10647, .F. ) ;
#19489 = CARTESIAN_POINT ( 'NONE',  ( 136.9269649396999853, -3660.140004248000423, 2250.236800000000130 ) ) ;
#19490 = ORIENTED_EDGE ( 'NONE', *, *, #12593, .T. ) ;
#19491 = ORIENTED_EDGE ( 'NONE', *, *, #11516, .T. ) ;
#19492 = SECURITY_CLASSIFICATION ( '', '', #15680 ) ;
#19493 = APPROVAL_PERSON_ORGANIZATION ( #13056, #23090, #2395 ) ;
#19494 = ORIENTED_EDGE ( 'NONE', *, *, #21693, .F. ) ;
#19495 = CARTESIAN_POINT ( 'NONE',  ( 47.95519999999999783, -3568.700000000000273, 2261.869999999999891 ) ) ;
#19496 = VERTEX_POINT ( 'NONE', #20162 ) ;
#19497 = ORIENTED_EDGE ( 'NONE', *, *, #531, .T. ) ;
#19498 = CARTESIAN_POINT ( 'NONE',  ( 4.926372769448470024, -3543.659322604134104, 2260.215249077962198 ) ) ;
#19499 = CALENDAR_DATE ( 2026, 26, 10 ) ;
#19500 = CARTESIAN_POINT ( 'NONE',  ( 117.9067999999989951, -3644.899999999999636, 2239.009999999999764 ) ) ;
#19501 = CYLINDRICAL_SURFACE ( 'NONE', #23043, 2.844799999998995244 ) ;
#19502 = ORIENTED_EDGE ( 'NONE', *, *, #16299, .T. ) ;
#19503 = AXIS2_PLACEMENT_3D ( 'NONE', #13643, #22079, #20446 ) ;
#19504 = CARTESIAN_POINT ( 'NONE',  ( 86.05520000000001346, -3594.099999999999909, 2259.837999999999738 ) ) ;
#19505 = FACE_OUTER_BOUND ( 'NONE', #20517, .T. ) ;
#19506 = DIRECTION ( 'NONE',  ( 0.000000000000000000, -1.000000000000000000, 0.000000000000000000 ) ) ;
#19507 = CARTESIAN_POINT ( 'NONE',  ( -6.349999999999999645, -3582.035000000000309, 2247.392000000000280 ) ) ;
#19508 = ORIENTED_EDGE ( 'NONE', *, *, #17026, .T. ) ;
#19509 = COORDINATED_UNIVERSAL_TIME_OFFSET ( 0, 0, .AHEAD. ) ;
#19510 = APPLIED_PERSON_AND_ORGANIZATION_ASSIGNMENT ( #18526, #2482, ( #7485 ) ) ;
#19511 = CARTESIAN_POINT ( 'NONE',  ( 131.8608732113245026, -3543.522855673919821, 2260.051190815687278 ) ) ;
#19512 = LOCAL_TIME ( 17, 37, 43.00000000000000000, #21616 ) ;
#19513 = LINE ( 'NONE', #10609, #17677 ) ;
#19514 = EDGE_CURVE ( 'NONE', #14916, #4467, #15526, .T. ) ;
#19515 = FACE_OUTER_BOUND ( 'NONE', #10730, .T. ) ;
#19516 = ORIENTED_EDGE ( 'NONE', *, *, #115, .T. ) ;
#19517 = VECTOR ( 'NONE', #9681, 1000.000000000000000 ) ;
#19518 = FACE_BOUND ( 'NONE', #9021, .T. ) ;
#19519 = EDGE_CURVE ( 'NONE', #18590, #10446, #15080, .T. ) ;
#19520 = CIRCLE ( 'NONE', #21766, 2.844799999999046758 ) ;
#19521 = DIRECTION ( 'NONE',  ( 0.000000000000000000, -1.000000000000000000, 0.000000000000000000 ) ) ;
#19522 = CARTESIAN_POINT ( 'NONE',  ( 145.2927459769028644, -3578.276998771325452, 2244.591060091298004 ) ) ;
#19523 = DIRECTION ( 'NONE',  ( -0.000000000000000000, -1.000000000000000000, -0.000000000000000000 ) ) ;
#19524 = CARTESIAN_POINT ( 'NONE',  ( 10.09961440033846181, -3660.701366163754301, 2250.195255585644190 ) ) ;
#19525 = ORIENTED_EDGE ( 'NONE', *, *, #2823, .T. ) ;
#19526 = CARTESIAN_POINT ( 'NONE',  ( 142.1895021645667327, -3658.067685255029119, 2239.009999999883348 ) ) ;
#19527 = ORIENTED_EDGE ( 'NONE', *, *, #15536, .T. ) ;
#19528 = CARTESIAN_POINT ( 'NONE',  ( 76.20000000000000284, -3670.300000000000182, 2239.771999999999935 ) ) ;
#19529 = CARTESIAN_POINT ( 'NONE',  ( 12.69999999997359197, -3636.810099999838712, 2296.433984632733427 ) ) ;
#19530 = CARTESIAN_POINT ( 'NONE',  ( 142.4730239663999782, -3578.859999866000180, 2250.236800057000437 ) ) ;
#19531 = CARTESIAN_POINT ( 'NONE',  ( 14.82309358269936261, -3657.611473550246956, 2248.695702319098473 ) ) ;
#19532 = CYLINDRICAL_SURFACE ( 'NONE', #19556, 2.844800000000001550 ) ;
#19533 = ORIENTED_EDGE ( 'NONE', *, *, #8556, .F. ) ;
#19534 = CARTESIAN_POINT ( 'NONE',  ( 9.926985991717000246, -3578.860012824000023, 2250.236835079999764 ) ) ;
#19535 = ORIENTED_EDGE ( 'NONE', *, *, #7069, .T. ) ;
#19536 = APPLIED_PERSON_AND_ORGANIZATION_ASSIGNMENT ( #1695, #8966, ( #20249 ) ) ;
#19537 = CIRCLE ( 'NONE', #451, 1.269999999999882334 ) ;
#19538 = CARTESIAN_POINT ( 'NONE',  ( 132.2269032045000188, -3544.443975155000317, 2260.454626673999883 ) ) ;
#19539 = B_SPLINE_CURVE_WITH_KNOTS ( 'NONE', 3,
 ( #1645, #1881, #9035, #134, #1773, #8917, #6936, #8802, #16062, #14429, #21580, #12082, #19352, #19235, #19466, #3168, #1418, #17579, #8574 ),
 .UNSPECIFIED., .F., .F.,
 ( 4, 1, 1, 1, 1, 1, 1, 1, 1, 1, 1, 1, 1, 1, 1, 1, 4 ),
 ( 0.000000000000000000, 0.06250000000000000000, 0.1250000000000000000, 0.1875000000000000000, 0.2500000000000000000, 0.3125000000000000000, 0.3750000000000000000, 0.4375000000000000000, 0.5000000000000000000, 0.5625000000000000000, 0.6250000000000000000, 0.6875000000000000000, 0.7500000000000000000, 0.8125000000000000000, 0.8750000000000000000, 0.9375000000000000000, 1.000000000000000000 ),
 .UNSPECIFIED. ) ;
#19540 = CARTESIAN_POINT ( 'NONE',  ( 12.69999999999999929, -3585.971999999999753, 2268.705139999999574 ) ) ;
#19541 = ITEM_DEFINED_TRANSFORMATION ( 'NONE', 'NONE', #8992,  #5611 ) ;
#19542 = CARTESIAN_POINT ( 'NONE',  ( 3.048000000000000043, -3694.938000000000102, 2238.248000000000047 ) ) ;
#19543 = EDGE_CURVE ( 'NONE', #17962, #15313, #13652, .T. ) ;
#19544 = CARTESIAN_POINT ( 'NONE',  ( 10.68485228337000059, -3657.490333022999948, 2257.776247070999943 ) ) ;
#19545 = DIRECTION ( 'NONE',  ( 0.000000000000000000, 0.000000000000000000, -1.000000000000000000 ) ) ;
#19546 = EDGE_CURVE ( 'NONE', #1150, #13971, #21487, .T. ) ;
#19547 = CIRCLE ( 'NONE', #13551, 0.7619999999999294005 ) ;
#19548 = DIRECTION ( 'NONE',  ( 1.000000000000000000, 0.000000000000000000, 0.000000000000000000 ) ) ;
#19549 = EDGE_CURVE ( 'NONE', #3918, #19866, #19644, .T. ) ;
#19550 = CARTESIAN_POINT ( 'NONE',  ( 17.37165482607458245, -3576.201487277430260, 2246.367956099597450 ) ) ;
#19551 = AXIS2_PLACEMENT_3D ( 'NONE', #14189, #19566, #22726 ) ;
#19552 = PLANE ( 'NONE',  #18121 ) ;
#19553 = ORIENTED_EDGE ( 'NONE', *, *, #3295, .T. ) ;
#19554 = AXIS2_PLACEMENT_3D ( 'NONE', #16484, #11105, #16147 ) ;
#19555 = DIRECTION ( 'NONE',  ( 1.224646799147353207E-16, 1.000000000000000000, -0.000000000000000000 ) ) ;
#19556 = AXIS2_PLACEMENT_3D ( 'NONE', #14268, #1954, #10508 ) ;
#19557 = CARTESIAN_POINT ( 'NONE',  ( 15.03168679717000167, -3660.851200000000063, 2239.391000000000076 ) ) ;
#19558 = VERTEX_POINT ( 'NONE', #16756 ) ;
#19559 = CARTESIAN_POINT ( 'NONE',  ( 116.8400000000000034, -3543.300000000000182, 2251.506800000000112 ) ) ;
#19560 = VERTEX_POINT ( 'NONE', #2003 ) ;
#19561 = DIRECTION ( 'NONE',  ( 1.000000000000000000, 0.000000000000000000, 0.000000000000000000 ) ) ;
#19562 = DIRECTION ( 'NONE',  ( 0.000000000000000000, -1.000000000000000000, 0.000000000000000000 ) ) ;
#19563 = ADVANCED_FACE ( 'NONE', ( #12895 ), #12535, .T. ) ;
#19564 = ORIENTED_EDGE ( 'NONE', *, *, #14814, .T. ) ;
#19565 = VERTEX_POINT ( 'NONE', #16293 ) ;
#19566 = DIRECTION ( 'NONE',  ( 0.000000000000000000, -2.336881798971000105E-14, 1.000000000000000000 ) ) ;
#19567 = ORIENTED_EDGE ( 'NONE', *, *, #7816, .T. ) ;
#19569 = CYLINDRICAL_SURFACE ( 'NONE', #1389, 2.844800000000091700 ) ;
#19568 = CIRCLE ( 'NONE', #22544, 0.7619999999999294005 ) ;
#19570 = PERSON_AND_ORGANIZATION ( #5446, #1895 ) ;
#19571 = AXIS2_PLACEMENT_3D ( 'NONE', #9283, #9043, #265 ) ;
#19572 = LINE ( 'NONE', #17920, #20947 ) ;
#19573 = FACE_OUTER_BOUND ( 'NONE', #7615, .T. ) ;
#19574 = CARTESIAN_POINT ( 'NONE',  ( 3.175000000265765010, -3543.615630734505430, 2275.001800000000003 ) ) ;
#19575 = ADVANCED_FACE ( 'NONE', ( #12664 ), #11419, .T. ) ;
#19576 = LINE ( 'NONE', #3513, #15096 ) ;
#19577 = DIRECTION ( 'NONE',  ( 0.000000000000000000, 0.000000000000000000, -1.000000000000000000 ) ) ;
#19578 = ORIENTED_EDGE ( 'NONE', *, *, #2060, .F. ) ;
#19579 = CIRCLE ( 'NONE', #3109, 0.7619999999999294005 ) ;
#19580 = CARTESIAN_POINT ( 'NONE',  ( 15.54875643158000642, -3695.598810868058536, 2255.000779105261699 ) ) ;
#19581 = ADVANCED_FACE ( 'NONE', ( #20276 ), #7324, .T. ) ;
#19582 = EDGE_CURVE ( 'NONE', #6627, #20964, #18900, .T. ) ;
#19583 = DIRECTION ( 'NONE',  ( 0.000000000000000000, 0.000000000000000000, -1.000000000000000000 ) ) ;
#19584 = ORIENTED_EDGE ( 'NONE', *, *, #2524, .F. ) ;
#19585 = CARTESIAN_POINT ( 'NONE',  ( 4.752492555451421907, -3695.617810901896064, 2259.779947940402053 ) ) ;
#19586 = CARTESIAN_POINT ( 'NONE',  ( 15.24000000000000021, -3544.570000000000164, 2255.774000000000342 ) ) ;
#19587 = AXIS2_PLACEMENT_3D ( 'NONE', #2837, #11618, #2718 ) ;
#19588 = TOROIDAL_SURFACE ( 'NONE', #4605, 4.114799999999999791, 1.270000000000000018 ) ;
#19589 = CARTESIAN_POINT ( 'NONE',  ( 116.8400000000000034, -3670.300000000000182, 2247.392000000000280 ) ) ;
#19590 = EDGE_LOOP ( 'NONE', ( #10368, #19122, #18076, #16265 ) ) ;
#19591 = DIRECTION ( 'NONE',  ( 0.000000000000000000, 0.000000000000000000, -1.000000000000000000 ) ) ;
#19592 = CARTESIAN_POINT ( 'NONE',  ( 73.35520000000001062, -3568.700000000000273, 2259.837999999999738 ) ) ;
#19593 = ORIENTED_EDGE ( 'NONE', *, *, #20313, .F. ) ;
#19594 = CARTESIAN_POINT ( 'NONE',  ( 25.39999999999999858, -3619.500000000000000, 2261.869999999999891 ) ) ;
#19595 = CARTESIAN_POINT ( 'NONE',  ( 11.47192027633000144, -3642.075229274999856, 2279.750852048000070 ) ) ;
#19596 = CARTESIAN_POINT ( 'NONE',  ( 18.03837739911582716, -3577.416356074214946, 2244.919848787751107 ) ) ;
#19597 = PLANE ( 'NONE',  #11135 ) ;
#19598 = AXIS2_PLACEMENT_3D ( 'NONE', #3371, #11072, #7447 ) ;
#19599 = EDGE_CURVE ( 'NONE', #3230, #22409, #12778, .T. ) ;
#19600 = DATE_TIME_ROLE ( 'classification_date' ) ;
#19601 = VERTEX_POINT ( 'NONE', #18164 ) ;
#19602 = FACE_OUTER_BOUND ( 'NONE', #7831, .T. ) ;
#19603 = CARTESIAN_POINT ( 'NONE',  ( 9.958250541862835092, -3695.444958116419457, 2255.268480149500647 ) ) ;
#19604 = ORIENTED_EDGE ( 'NONE', *, *, #22684, .F. ) ;
#19605 = DIRECTION ( 'NONE',  ( 0.000000000000000000, -1.000000000000000000, 0.000000000000000000 ) ) ;
#19606 = CARTESIAN_POINT ( 'NONE',  ( 137.9036726380650748, -3657.299095976264653, 2247.222869807297684 ) ) ;
#19607 = ORIENTED_EDGE ( 'NONE', *, *, #19022, .T. ) ;
#19608 = DIRECTION ( 'NONE',  ( -1.000000000000000000, 0.000000000000000000, 0.000000000000000000 ) ) ;
#19609 = ADVANCED_FACE ( 'NONE', ( #2123 ), #2235, .T. ) ;
#19610 = ORIENTED_EDGE ( 'NONE', *, *, #2958, .F. ) ;
#19611 = ORIENTED_EDGE ( 'NONE', *, *, #19172, .T. ) ;
#19612 = ORIENTED_EDGE ( 'NONE', *, *, #7805, .T. ) ;
#19613 = CIRCLE ( 'NONE', #7630, 0.7619999999999294005 ) ;
#19614 = DIRECTION ( 'NONE',  ( 0.000000000000000000, 2.336881798971000105E-14, 1.000000000000000000 ) ) ;
#19615 = ORIENTED_EDGE ( 'NONE', *, *, #248, .F. ) ;
#19616 = ORIENTED_EDGE ( 'NONE', *, *, #746, .T. ) ;
#19617 = CARTESIAN_POINT ( 'NONE',  ( 4.752632297182751486, -3543.382189098389972, 2259.779892145590566 ) ) ;
#19618 = CONTEXT_DEPENDENT_SHAPE_REPRESENTATION ( #14149, #22301 ) ;
#19619 = CARTESIAN_POINT ( 'NONE',  ( -6.349999999999999645, -3578.860000000000127, 2247.392000000000280 ) ) ;
#19620 = CARTESIAN_POINT ( 'NONE',  ( 151.4000000000000057, -3694.430000000000291, 2260.570967364599255 ) ) ;
#19621 = VERTEX_POINT ( 'NONE', #16519 ) ;
#19622 = DIRECTION ( 'NONE',  ( 0.000000000000000000, 0.000000000000000000, -1.000000000000000000 ) ) ;
#19623 = DIRECTION ( 'NONE',  ( 0.000000000000000000, 1.000000000000000000, 0.000000000000000000 ) ) ;
#19624 = FACE_OUTER_BOUND ( 'NONE', #20998, .T. ) ;
#19625 = CARTESIAN_POINT ( 'NONE',  ( -8.890000000036000216, -3661.486200000000281, 2245.060313203000078 ) ) ;
#19626 = EDGE_CURVE ( 'NONE', #16091, #8900, #4681, .T. ) ;
#19627 = COORDINATED_UNIVERSAL_TIME_OFFSET ( 0, 0, .AHEAD. ) ;
#19628 = LINE ( 'NONE', #17748, #2675 ) ;
#19629 = AXIS2_PLACEMENT_3D ( 'NONE', #20354, #6069, #16825 ) ;
#19630 = CARTESIAN_POINT ( 'NONE',  ( 12.69999999999999929, -3579.494999999999891, 2245.359999999999673 ) ) ;
#19631 = CARTESIAN_POINT ( 'NONE',  ( 10.36831320285999958, -3660.851200000000063, 2242.820000000000164 ) ) ;
#19632 = CIRCLE ( 'NONE', #14770, 3.606800000000000228 ) ;
#19633 = ORIENTED_EDGE ( 'NONE', *, *, #15254, .F. ) ;
#19634 = DIRECTION ( 'NONE',  ( 0.000000000000000000, 0.000000000000000000, -1.000000000000000000 ) ) ;
#19635 = DIRECTION ( 'NONE',  ( -1.224646799141892071E-16, -1.000000000000000000, 2.336881798971000421E-14 ) ) ;
#19636 = CARTESIAN_POINT ( 'NONE',  ( 144.4597169060923534, -3576.330748743867389, 2246.087205944029847 ) ) ;
#19637 = FACE_OUTER_BOUND ( 'NONE', #13595, .T. ) ;
#19638 = FACE_OUTER_BOUND ( 'NONE', #16687, .T. ) ;
#19639 = ORIENTED_EDGE ( 'NONE', *, *, #7034, .F. ) ;
#19640 = CARTESIAN_POINT ( 'NONE',  ( 18.22188905710634899, -3658.031438926708688, 2245.481214767577967 ) ) ;
#19641 = ORIENTED_EDGE ( 'NONE', *, *, #10388, .T. ) ;
#19642 = TOROIDAL_SURFACE ( 'NONE', #14835, 4.114799999999999791, 1.270000000000000018 ) ;
#19643 = DIRECTION ( 'NONE',  ( 0.000000000000000000, 0.000000000000000000, -1.000000000000000000 ) ) ;
#19644 = CIRCLE ( 'NONE', #9536, 5.080000000000000071 ) ;
#19645 = PLANE ( 'NONE',  #6588 ) ;
#19646 = AXIS2_PLACEMENT_3D ( 'NONE', #21323, #23060, #10768 ) ;
#19647 = APPLICATION_CONTEXT ( 'configuration controlled 3d designs of mechanical parts and assemblies' ) ;
#19648 = DIRECTION ( 'NONE',  ( 0.000000000000000000, 1.000000000000000000, 0.000000000000000000 ) ) ;
#19649 = AXIS2_PLACEMENT_3D ( 'NONE', #7888, #9863, #18656 ) ;
#19650 = CARTESIAN_POINT ( 'NONE',  ( 14.65200945848731351, -3657.435257283903866, 2248.274806926763176 ) ) ;
#19651 = DIRECTION ( 'NONE',  ( 0.000000000000000000, 0.000000000000000000, 1.000000000000000000 ) ) ;
#19652 = VERTEX_POINT ( 'NONE', #11696 ) ;
#19653 = CARTESIAN_POINT ( 'NONE',  ( 12.69999999999999929, -3579.494999999999891, 2270.760000000000218 ) ) ;
#19654 = ORIENTED_EDGE ( 'NONE', *, *, #10388, .F. ) ;
#19655 = DIRECTION ( 'NONE',  ( 0.000000000000000000, -2.848874176402999842E-12, 1.000000000000000000 ) ) ;
#19656 = FACE_OUTER_BOUND ( 'NONE', #4112, .T. ) ;
#19657 = APPROVAL_DATE_TIME ( #19316, #16776 ) ;
#19658 = DIRECTION ( 'NONE',  ( -1.000000000000000000, 0.000000000000000000, 0.000000000000000000 ) ) ;
#19659 = DIRECTION ( 'NONE',  ( 0.000000000000000000, -1.000000000000000000, 0.000000000000000000 ) ) ;
#19660 = CARTESIAN_POINT ( 'NONE',  ( 151.1299999999999955, -3543.299999999999727, 2259.329999999999927 ) ) ;
#19661 = AXIS2_PLACEMENT_3D ( 'NONE', #16555, #15265, #507 ) ;
#19662 = AXIS2_PLACEMENT_3D ( 'NONE', #17552, #1499, #23058 ) ;
#19663 = CARTESIAN_POINT ( 'NONE',  ( 12.70000000000000107, -3590.289999999999964, 2279.817639999999756 ) ) ;
#19664 = AXIS2_PLACEMENT_3D ( 'NONE', #18826, #780, #11666 ) ;
#19665 = CIRCLE ( 'NONE', #9558, 2.844800000000091700 ) ;
#19666 = ORIENTED_EDGE ( 'NONE', *, *, #17016, .F. ) ;
#19667 = CARTESIAN_POINT ( 'NONE',  ( 50.79999999999999716, -3670.300000000000182, 2259.837999999999738 ) ) ;
#19668 = VERTEX_POINT ( 'NONE', #4333 ) ;
#19669 = FACE_OUTER_BOUND ( 'NONE', #16454, .T. ) ;
#19670 = APPLIED_PERSON_AND_ORGANIZATION_ASSIGNMENT ( #14819, #18552, ( #16085 ) ) ;
#19671 = DIRECTION ( 'NONE',  ( -1.000000000000000000, 0.000000000000000000, 0.000000000000000000 ) ) ;
#19672 = ADVANCED_FACE ( 'NONE', ( #15458 ), #1035, .T. ) ;
#19673 = ORIENTED_EDGE ( 'NONE', *, *, #2549, .F. ) ;
#19674 = CARTESIAN_POINT ( 'NONE',  ( 12.69999999999999929, -3585.210000000000036, 2263.117139999999836 ) ) ;
#19675 = ADVANCED_FACE ( 'NONE', ( #17202 ), #20408, .T. ) ;
#19676 = ORIENTED_EDGE ( 'NONE', *, *, #17890, .T. ) ;
#19677 = CARTESIAN_POINT ( 'NONE',  ( 142.2521248979318784, -3694.709202398072648, 2255.743570596264817 ) ) ;
#19678 = DIRECTION ( 'NONE',  ( 0.000000000000000000, 0.000000000000000000, 1.000000000000000000 ) ) ;
#19679 = EDGE_CURVE ( 'NONE', #6461, #20178, #16974, .T. ) ;
#19680 = CIRCLE ( 'NONE', #22653, 5.460999999999938126 ) ;
#19681 = CIRCLE ( 'NONE', #1711, 0.7619999999999294005 ) ;
#19682 = VERTEX_POINT ( 'NONE', #22240 ) ;
#19683 = PRODUCT_DEFINITION_SHAPE ( 'NONE', 'NONE',  #11226 ) ;
#19684 = EDGE_CURVE ( 'NONE', #6769, #17073, #2821, .T. ) ;
#19685 =( REPRESENTATION_RELATIONSHIP ('NONE','NONE', #20448, #16547 ) REPRESENTATION_RELATIONSHIP_WITH_TRANSFORMATION ( #17857 )SHAPE_REPRESENTATION_RELATIONSHIP( ) );
#19686 = AXIS2_PLACEMENT_3D ( 'NONE', #17661, #15334, #13695 ) ;
#19687 = AXIS2_PLACEMENT_3D ( 'NONE', #9242, #4075, #10994 ) ;
#19688 = CARTESIAN_POINT ( 'NONE',  ( 137.5277363187835249, -3581.332105450641393, 2248.799968448360687 ) ) ;
#19689 = ORIENTED_EDGE ( 'NONE', *, *, #4385, .T. ) ;
#19690 = CARTESIAN_POINT ( 'NONE',  ( 142.7470794804999912, -3543.299999999999727, 2254.503999999999905 ) ) ;
#19691 = CIRCLE ( 'NONE', #9577, 2.844800000000091700 ) ;
#19692 = CALENDAR_DATE ( 2026, 26, 10 ) ;
#19693 = VECTOR ( 'NONE', #6456, 1000.000000000000000 ) ;
#19694 = CYLINDRICAL_SURFACE ( 'NONE', #18333, 11.11249999999985860 ) ;
#19695 = ADVANCED_FACE ( 'NONE', ( #9716 ), #8195, .T. ) ;
#19696 = DIRECTION ( 'NONE',  ( 1.000000000000000000, 0.000000000000000000, 0.000000000000000000 ) ) ;
#19697 = CARTESIAN_POINT ( 'NONE',  ( 2.859369265602505816, -3543.299999999999727, 2275.763800000000629 ) ) ;
#19698 = CARTESIAN_POINT ( 'NONE',  ( 12.69999999999999929, -3639.502500000000055, 2290.241799999999785 ) ) ;
#19699 = CIRCLE ( 'NONE', #8837, 0.3810000000000002829 ) ;
#19700 = EDGE_CURVE ( 'NONE', #8573, #21672, #21174, .T. ) ;
#19701 = DIRECTION ( 'NONE',  ( 0.000000000000000000, 0.000000000000000000, -1.000000000000000000 ) ) ;
#19702 = EDGE_LOOP ( 'NONE', ( #20903, #4964, #17309, #9244, #9723, #10119 ) ) ;
#19703 = VECTOR ( 'NONE', #6736, 1000.000000000000114 ) ;
#19704 = CARTESIAN_POINT ( 'NONE',  ( 134.0212987838334584, -3578.851531742024690, 2244.547209130087140 ) ) ;
#19705 = CIRCLE ( 'NONE', #9593, 0.7619999999999294005 ) ;
#19706 = DIRECTION ( 'NONE',  ( 0.000000000000000000, -1.000000000000000000, 0.000000000000000000 ) ) ;
#19707 = VERTEX_POINT ( 'NONE', #9939 ) ;
#19708 = CARTESIAN_POINT ( 'NONE',  ( 4.891028678428722465, -3695.419680866766612, 2260.126887239455755 ) ) ;
#19709 = DIRECTION ( 'NONE',  ( -0.000000000000000000, 1.224646799147353207E-16, 1.000000000000000000 ) ) ;
#19710 =( BOUNDED_CURVE ( )  B_SPLINE_CURVE ( 3, ( #20003, #5941, #18344, #14844 ),
 .UNSPECIFIED., .F., .T. ) 
 B_SPLINE_CURVE_WITH_KNOTS ( ( 4, 4 ),
 ( 1.570796326606976656, 3.141592653589793116 ),
 .UNSPECIFIED. ) 
 CURVE ( )  GEOMETRIC_REPRESENTATION_ITEM ( )  RATIONAL_B_SPLINE_CURVE ( ( 1.000000000000000000, 0.8047378540800718127, 0.8047378540800718127, 1.000000000000000000 ) ) 
 REPRESENTATION_ITEM ( '' )  );
#19711 = CARTESIAN_POINT ( 'NONE',  ( 152.4000000000000057, -3694.938000000000102, 2275.763800000000174 ) ) ;
#19712 = EDGE_LOOP ( 'NONE', ( #1016, #10449, #4372, #22876, #17732 ) ) ;
#19713 = CARTESIAN_POINT ( 'NONE',  ( 15.53591867179932073, -3659.780168290938946, 2257.960586820520803 ) ) ;
#19714 = DIRECTION ( 'NONE',  ( -1.000000000000000000, 2.330758767201999921E-14, 2.343004830739999973E-14 ) ) ;
#19715 = ORIENTED_EDGE ( 'NONE', *, *, #1097, .T. ) ;
#19716 = ADVANCED_FACE ( 'NONE', ( #6330 ), #13586, .F. ) ;
#19717 = CARTESIAN_POINT ( 'NONE',  ( -5.588000000000000078, -3694.938000000000102, 2253.487999999999829 ) ) ;
#19718 = CARTESIAN_POINT ( 'NONE',  ( 15.47299515201000020, -3578.859991782000179, 2250.236800948000109 ) ) ;
#19719 = DIRECTION ( 'NONE',  ( 0.000000000000000000, 1.000000000000000000, 0.000000000000000000 ) ) ;
#19720 = CARTESIAN_POINT ( 'NONE',  ( 129.8447999999989975, -3670.300000000000182, 2261.869999999999891 ) ) ;
#19721 = CALENDAR_DATE ( 2026, 26, 10 ) ;
#19722 = AXIS2_PLACEMENT_3D ( 'NONE', #19251, #15736, #3653 ) ;
#19723 = CARTESIAN_POINT ( 'NONE',  ( 136.9873132028999976, -3661.071170452878050, 2239.009999999999764 ) ) ;
#19724 = DIRECTION ( 'NONE',  ( 0.000000000000000000, 0.000000000000000000, 1.000000000000000000 ) ) ;
#19725 = ORIENTED_EDGE ( 'NONE', *, *, #11173, .T. ) ;
#19726 = CYLINDRICAL_SURFACE ( 'NONE', #9248, 5.715000000000001634 ) ;
#19727 = ADVANCED_BREP_SHAPE_REPRESENTATION ( '', ( #13372, #5611 ), #13859 ) ;
#19728 = AXIS2_PLACEMENT_3D ( 'NONE', #6928, #16288, #247 ) ;
#19729 = CARTESIAN_POINT ( 'NONE',  ( 137.8417952671095179, -3657.349591785569828, 2246.808273363673834 ) ) ;
#19730 = EDGE_LOOP ( 'NONE', ( #922, #17203, #14012, #4172 ) ) ;
#19731 = CYLINDRICAL_SURFACE ( 'NONE', #10359, 0.7620000000000001217 ) ;
#19732 = VERTEX_POINT ( 'NONE', #2795 ) ;
#19733 = ORIENTED_EDGE ( 'NONE', *, *, #10784, .F. ) ;
#19734 = ORIENTED_EDGE ( 'NONE', *, *, #18673, .F. ) ;
#19735 = AXIS2_PLACEMENT_3D ( 'NONE', #7179, #12682, #14447 ) ;
#19736 = DIRECTION ( 'NONE',  ( 0.000000000000000000, 1.000000000000000000, 0.000000000000000000 ) ) ;
#19737 = EDGE_LOOP ( 'NONE', ( #23148, #20657, #11457, #8971 ) ) ;
#19738 = ORIENTED_EDGE ( 'NONE', *, *, #17163, .F. ) ;
#19739 = CYLINDRICAL_SURFACE ( 'NONE', #22863, 2.844799999998998796 ) ;
#19740 = CALENDAR_DATE ( 2026, 26, 10 ) ;
#19741 = DIRECTION ( 'NONE',  ( -1.000000000000000000, 0.000000000000000000, 0.000000000000000000 ) ) ;
#19742 = DIRECTION ( 'NONE',  ( -1.000000000000000000, 0.000000000000000000, 0.000000000000000000 ) ) ;
#19743 = ORIENTED_EDGE ( 'NONE', *, *, #8824, .T. ) ;
#19744 = AXIS2_PLACEMENT_3D ( 'NONE', #12862, #9462, #12982 ) ;
#19745 = PLANE ( 'NONE',  #13711 ) ;
#19746 = AXIS2_PLACEMENT_3D ( 'NONE', #9509, #22039, #13138 ) ;
#19747 = DIRECTION ( 'NONE',  ( 0.000000000000000000, 0.000000000000000000, 1.000000000000000000 ) ) ;
#19748 = CARTESIAN_POINT ( 'NONE',  ( 9.855200508358999301, -3579.494990670147217, 2257.962940201000038 ) ) ;
#19749 = CARTESIAN_POINT ( 'NONE',  ( 142.0316867971999955, -3655.466399999999794, 2242.820000000000164 ) ) ;
#19750 = CALENDAR_DATE ( 2026, 26, 10 ) ;
#19751 = EDGE_CURVE ( 'NONE', #22138, #18199, #20851, .T. ) ;
#19752 = EDGE_CURVE ( 'NONE', #20464, #565, #19297, .T. ) ;
#19753 = ORIENTED_EDGE ( 'NONE', *, *, #5687, .T. ) ;
#19754 = CARTESIAN_POINT ( 'NONE',  ( 131.7615871309722877, -3543.390959416002715, 2259.802598284109536 ) ) ;
#19755 = ADVANCED_FACE ( 'NONE', ( #6445 ), #18977, .F. ) ;
#19756 = VERTEX_POINT ( 'NONE', #20605 ) ;
#19757 = CARTESIAN_POINT ( 'NONE',  ( 12.69999999999999929, -3659.504999999999654, 2255.774000000000342 ) ) ;
#19758 = TOROIDAL_SURFACE ( 'NONE', #20142, 1.524000000000000021, 0.7620000000000000107 ) ;
#19759 = DIRECTION ( 'NONE',  ( 0.000000000000000000, 0.000000000000000000, -1.000000000000000000 ) ) ;
#19760 = EDGE_CURVE ( 'NONE', #19668, #22154, #21902, .T. ) ;
#19761 = ORIENTED_EDGE ( 'NONE', *, *, #9271, .F. ) ;
#19762 = FACE_BOUND ( 'NONE', #20669, .T. ) ;
#19763 = TOROIDAL_SURFACE ( 'NONE', #1033, 3.606799999999999784, 0.7620000000000000107 ) ;
#19764 = FACE_OUTER_BOUND ( 'NONE', #13884, .T. ) ;
#19765 = CARTESIAN_POINT ( 'NONE',  ( 144.7935381745138557, -3576.902450837929791, 2245.303073078667239 ) ) ;
#19766 = CARTESIAN_POINT ( 'NONE',  ( 12.69999999999999929, -3585.210000000000036, 2268.705139999999574 ) ) ;
#19767 = EDGE_CURVE ( 'NONE', #17500, #18712, #8313, .T. ) ;
#19768 = CARTESIAN_POINT ( 'NONE',  ( 139.6999999999999886, -3579.494999999999891, 2270.760000000000218 ) ) ;
#19769 = EDGE_CURVE ( 'NONE', #6778, #2966, #22591, .T. ) ;
#19770 = CARTESIAN_POINT ( 'NONE',  ( 18.11987658286814096, -3657.692177165366502, 2245.942492754456453 ) ) ;
#19771 = ORIENTED_EDGE ( 'NONE', *, *, #15419, .F. ) ;
#19772 = CARTESIAN_POINT ( 'NONE',  ( 147.4569508202075383, -3695.298184790736741, 2260.256966980285142 ) ) ;
#19773 = DIRECTION ( 'NONE',  ( 0.000000000000000000, 0.000000000000000000, 1.000000000000000000 ) ) ;
#19774 = CARTESIAN_POINT ( 'NONE',  ( 12.70000000000085727, -3636.657698770567094, 2279.817639764978139 ) ) ;
#19775 = CIRCLE ( 'NONE', #1048, 3.606800000000021100 ) ;
#19776 = FACE_OUTER_BOUND ( 'NONE', #21972, .T. ) ;
#19777 = CARTESIAN_POINT ( 'NONE',  ( 142.5057674346834915, -3543.452888078422802, 2255.108514515849038 ) ) ;
#19778 = CARTESIAN_POINT ( 'NONE',  ( 110.6932000000009992, -3644.899999999999636, 2259.837999999999738 ) ) ;
#19779 = CARTESIAN_POINT ( 'NONE',  ( 7.661546442962579029, -3576.797734221649080, 2245.432411850466451 ) ) ;
#19780 = ORIENTED_EDGE ( 'NONE', *, *, #12109, .F. ) ;
#19781 = CARTESIAN_POINT ( 'NONE',  ( 12.69999999999999929, -3657.599999999999909, 2270.760000000000218 ) ) ;
#19782 = CARTESIAN_POINT ( 'NONE',  ( 20.32000000000000028, -3543.299999999999727, 2289.213099999999940 ) ) ;
#19783 = DATE_AND_TIME ( #9345, #7900 ) ;
#19784 = FACE_OUTER_BOUND ( 'NONE', #4730, .T. ) ;
#19785 = CARTESIAN_POINT ( 'NONE',  ( 10.89511648704999836, -3657.299999577000108, 2257.739442794000297 ) ) ;
#19786 = DIRECTION ( 'NONE',  ( 0.000000000000000000, 0.000000000000000000, -1.000000000000000000 ) ) ;
#19787 = LINE ( 'NONE', #19663, #4031 ) ;
#19788 = ORIENTED_EDGE ( 'NONE', *, *, #17985, .F. ) ;
#19789 = CARTESIAN_POINT ( 'NONE',  ( 3.048000000000000043, -3695.699999999999818, 2238.248000000000047 ) ) ;
#19790 = ORIENTED_EDGE ( 'NONE', *, *, #9768, .T. ) ;
#19791 = DIRECTION ( 'NONE',  ( -1.000000000000000000, 0.000000000000000000, 0.000000000000000000 ) ) ;
#19792 = CYLINDRICAL_SURFACE ( 'NONE', #20425, 1.269999999999900320 ) ;
#19793 = EDGE_LOOP ( 'NONE', ( #7251, #22146, #11395, #17961, #7628, #7274 ) ) ;
#19794 = DIRECTION ( 'NONE',  ( 0.000000000000000000, -1.000000000000000000, 0.000000000000000000 ) ) ;
#19795 = ORIENTED_EDGE ( 'NONE', *, *, #17820, .T. ) ;
#19796 = CARTESIAN_POINT ( 'NONE',  ( 142.3802386003915785, -3695.306816721881205, 2255.422803181790186 ) ) ;
#19797 = CARTESIAN_POINT ( 'NONE',  ( 76.20000000000000284, -3568.700000000000273, 2239.771999999999935 ) ) ;
#19798 = ORIENTED_EDGE ( 'NONE', *, *, #11880, .T. ) ;
#19799 = ORIENTED_EDGE ( 'NONE', *, *, #9265, .F. ) ;
#19800 = CARTESIAN_POINT ( 'NONE',  ( 137.2808927978301199, -3580.991830095288151, 2249.275667250868992 ) ) ;
#19801 = ORIENTED_EDGE ( 'NONE', *, *, #7931, .T. ) ;
#19802 = VECTOR ( 'NONE', #19065, 1000.000000000000000 ) ;
#19803 = DIRECTION ( 'NONE',  ( 0.000000000000000000, -1.000000000000000000, 0.000000000000000000 ) ) ;
#19804 = COORDINATED_UNIVERSAL_TIME_OFFSET ( 0, 0, .AHEAD. ) ;
#19805 = APPROVAL ( #2334, 'UNSPECIFIED' ) ;
#19806 = CARTESIAN_POINT ( 'NONE',  ( 56.10057940168000812, -3544.061999999999898, 2275.211350432000472 ) ) ;
#19807 = SPHERICAL_SURFACE ( 'NONE', #12991, 1.270000000000000018 ) ;
#19808 = SPHERICAL_SURFACE ( 'NONE', #15216, 0.7620000000000000107 ) ;
#19809 = CARTESIAN_POINT ( 'NONE',  ( 20.62424768829000143, -3694.430000000000291, 2260.600000000000364 ) ) ;
#19810 = EDGE_CURVE ( 'NONE', #15062, #16201, #15115, .T. ) ;
#19811 = ADVANCED_FACE ( 'NONE', ( #20496 ), #1315, .T. ) ;
#19812 = CARTESIAN_POINT ( 'NONE',  ( 138.9181842230315738, -3576.759674807602096, 2249.310742386851871 ) ) ;
#19813 = ORIENTED_EDGE ( 'NONE', *, *, #13156, .F. ) ;
#19814 = CARTESIAN_POINT ( 'NONE',  ( 142.2400000000000091, -3578.213872745999652, 2255.774000000000342 ) ) ;
#19815 = AXIS2_PLACEMENT_3D ( 'NONE', #15191, #11653, #18811 ) ;
#19816 = EDGE_CURVE ( 'NONE', #2067, #6140, #11580, .T. ) ;
#19817 = ORIENTED_EDGE ( 'NONE', *, *, #2060, .T. ) ;
#19818 = ORIENTED_EDGE ( 'NONE', *, *, #8570, .F. ) ;
#19819 = CARTESIAN_POINT ( 'NONE',  ( 11.88126810894999963, -3582.224158427000020, 2257.621768944999985 ) ) ;
#19820 = ORIENTED_EDGE ( 'NONE', *, *, #18146, .F. ) ;
#19821 = CIRCLE ( 'NONE', #22789, 2.844799999999999773 ) ;
#19822 = DIRECTION ( 'NONE',  ( 0.000000000000000000, -1.000000000000000000, 0.000000000000000000 ) ) ;
#19823 = EDGE_LOOP ( 'NONE', ( #4019, #10213, #18763, #21563, #2327 ) ) ;
#19824 = CARTESIAN_POINT ( 'NONE',  ( 13.78126912685999983, -3662.141243252000095, 2257.644351290000031 ) ) ;
#19825 = CARTESIAN_POINT ( 'NONE',  ( 12.70000000000000107, -3649.471999999999753, 2275.817139999999654 ) ) ;
#19826 = ORIENTED_EDGE ( 'NONE', *, *, #10057, .F. ) ;
#19827 = DIRECTION ( 'NONE',  ( 0.000000000000000000, 1.000000000000000000, 0.000000000000000000 ) ) ;
#19828 = FACE_BOUND ( 'NONE', #3946, .T. ) ;
#19829 = DIRECTION ( 'NONE',  ( 0.000000000000000000, 0.000000000000000000, 1.000000000000000000 ) ) ;
#19830 = DATE_AND_TIME ( #18069, #7124 ) ;
#19831 = CARTESIAN_POINT ( 'NONE',  ( 12.69999999997567208, -3642.194900000083180, 2296.210799999999836 ) ) ;
#19832 = CARTESIAN_POINT ( 'NONE',  ( 76.20000000000000284, -3670.300000000000182, 2239.771999999999935 ) ) ;
#19833 = ORIENTED_EDGE ( 'NONE', *, *, #3930, .F. ) ;
#19834 = LOCAL_TIME ( 17, 37, 43.00000000000000000, #3306 ) ;
#19835 = CARTESIAN_POINT ( 'NONE',  ( 18.03606895320094594, -3581.542328871593327, 2246.419514926349166 ) ) ;
#19836 = CIRCLE ( 'NONE', #16087, 0.7619999999999294005 ) ;
#19837 = CARTESIAN_POINT ( 'NONE',  ( 137.4930112367257209, -3657.709449394080366, 2248.871353917016677 ) ) ;
#19838 = EDGE_CURVE ( 'NONE', #5090, #22478, #20056, .T. ) ;
#19839 = ORIENTED_EDGE ( 'NONE', *, *, #4360, .F. ) ;
#19840 = SHAPE_REPRESENTATION ( 'Screw 6', ( #5611 ), #12740 ) ;
#19841 = EDGE_CURVE ( 'NONE', #2161, #16552, #20775, .T. ) ;
#19842 = CARTESIAN_POINT ( 'NONE',  ( 138.5760044042908987, -3662.119678798826499, 2249.435431913212142 ) ) ;
#19843 = EDGE_CURVE ( 'NONE', #15258, #5300, #11060, .T. ) ;
#19844 = EDGE_LOOP ( 'NONE', ( #15397, #15485 ) ) ;
#19845 = EDGE_LOOP ( 'NONE', ( #15725, #6649, #20310, #11568 ) ) ;
#19846 = ORIENTED_EDGE ( 'NONE', *, *, #4777, .F. ) ;
#19847 = VECTOR ( 'NONE', #7246, 1000.000000000000000 ) ;
#19848 = FACE_OUTER_BOUND ( 'NONE', #1682, .T. ) ;
#19849 = ORIENTED_EDGE ( 'NONE', *, *, #281, .T. ) ;
#19850 = ORIENTED_EDGE ( 'NONE', *, *, #5288, .F. ) ;
#19851 = ORGANIZATION ( 'NAUO-ORG2', 'UNSPECIFIED', 'UNSPECIFIED' ) ;
#19852 = CARTESIAN_POINT ( 'NONE',  ( 12.69999999976711180, -3582.627340905157780, 2239.009999999999764 ) ) ;
#19853 = DIRECTION ( 'NONE',  ( -1.000000000000000000, 0.000000000000000000, 0.000000000000000000 ) ) ;
#19854 = CYLINDRICAL_SURFACE ( 'NONE', #6324, 0.7619999999999294005 ) ;
#19855 = ORIENTED_EDGE ( 'NONE', *, *, #15390, .T. ) ;
#19856 = DIRECTION ( 'NONE',  ( 0.000000000000000000, 0.000000000000000000, 1.000000000000000000 ) ) ;
#19857 = FACE_OUTER_BOUND ( 'NONE', #283, .T. ) ;
#19858 = LINE ( 'NONE', #16341, #14728 ) ;
#19859 = AXIS2_PLACEMENT_3D ( 'NONE', #21699, #9284, #7408 ) ;
#19860 = ADVANCED_FACE ( 'NONE', ( #6794 ), #13669, .T. ) ;
#19861 = PLANE ( 'NONE',  #14490 ) ;
#19862 = COORDINATED_UNIVERSAL_TIME_OFFSET ( 0, 0, .AHEAD. ) ;
#19863 = DIRECTION ( 'NONE',  ( -1.000000000000000000, 0.000000000000000000, 0.000000000000000000 ) ) ;
#19864 = ORIENTED_EDGE ( 'NONE', *, *, #20568, .F. ) ;
#19865 = CARTESIAN_POINT ( 'NONE',  ( 137.1599999999999966, -3544.570000000000164, 2255.774000000000342 ) ) ;
#19866 = VERTEX_POINT ( 'NONE', #5384 ) ;
#19867 = CARTESIAN_POINT ( 'NONE',  ( 127.0000000000000000, -3619.500000000000000, 2259.837999999999738 ) ) ;
#19868 = DIRECTION ( 'NONE',  ( 1.000000000000000000, 0.000000000000000000, 0.000000000000000000 ) ) ;
#19869 = ORIENTED_EDGE ( 'NONE', *, *, #4910, .T. ) ;
#19870 = ORIENTED_EDGE ( 'NONE', *, *, #7994, .F. ) ;
#19871 = PLANE ( 'NONE',  #11445 ) ;
#19872 = EDGE_CURVE ( 'NONE', #11827, #7259, #10531, .T. ) ;
#19873 = DIRECTION ( 'NONE',  ( 0.000000000000000000, 0.000000000000000000, -1.000000000000000000 ) ) ;
#19874 = CARTESIAN_POINT ( 'NONE',  ( 10.36831320289432057, -3600.843700000111312, 2296.210799999999836 ) ) ;
#19875 = DIRECTION ( 'NONE',  ( 2.324635735433000053E-14, 0.000000000000000000, 1.000000000000000000 ) ) ;
#19876 = ADVANCED_FACE ( 'NONE', ( #14286 ), #10643, .F. ) ;
#19877 = AXIS2_PLACEMENT_3D ( 'NONE', #10853, #3699, #20117 ) ;
#19878 = EDGE_CURVE ( 'NONE', #3857, #8367, #16298, .T. ) ;
#19879 = CARTESIAN_POINT ( 'NONE',  ( 18.07700247900687529, -3657.567912637663994, 2246.174638830017102 ) ) ;
#19880 = EDGE_LOOP ( 'NONE', ( #14411, #15567, #8063, #5502 ) ) ;
#19881 = CARTESIAN_POINT ( 'NONE',  ( 147.3682464508232783, -3694.976217803879081, 2260.479245238027033 ) ) ;
#19882 = DIRECTION ( 'NONE',  ( 1.000000000000000000, 0.000000000000000000, 0.000000000000000000 ) ) ;
#19883 = PLANE ( 'NONE',  #960 ) ;
#19884 = CARTESIAN_POINT ( 'NONE',  ( 105.2067999999999870, -3619.500000000000000, 2259.837999999999738 ) ) ;
#19885 = CARTESIAN_POINT ( 'NONE',  ( 142.3627463449352604, -3543.741058433257422, 2255.466568423349599 ) ) ;
#19886 = CARTESIAN_POINT ( 'NONE',  ( 12.69999999994000106, -3596.805100000000039, 2292.781800000000203 ) ) ;
#19887 = APPLIED_SECURITY_CLASSIFICATION_ASSIGNMENT ( #15394, ( #23177 ) ) ;
#19888 = ADVANCED_FACE ( 'NONE', ( #3610 ), #14054, .T. ) ;
#19889 = CARTESIAN_POINT ( 'NONE',  ( 7.831451107590767791, -3576.501952514877757, 2245.800612488090792 ) ) ;
#19890 = VERTEX_POINT ( 'NONE', #7035 ) ;
#19891 = DATE_TIME_ROLE ( 'classification_date' ) ;
#19892 = DIRECTION ( 'NONE',  ( -0.000000000000000000, -1.000000000000000000, -0.000000000000000000 ) ) ;
#19893 = CARTESIAN_POINT ( 'NONE',  ( 139.7000000001000046, -3576.802599999999984, 2239.391000000000076 ) ) ;
#19894 = CIRCLE ( 'NONE', #3421, 1.269999999999882334 ) ;
#19895 = CONTEXT_DEPENDENT_SHAPE_REPRESENTATION ( #1716, #7723 ) ;
#19896 = ADVANCED_FACE ( 'NONE', ( #15927 ), #9554, .T. ) ;
#19897 = AXIS2_PLACEMENT_3D ( 'NONE', #5414, #11026, #12672 ) ;
#19898 = DIRECTION ( 'NONE',  ( 1.000000000000000000, 0.000000000000000000, 0.000000000000000000 ) ) ;
#19899 = EDGE_CURVE ( 'NONE', #10930, #6730, #15579, .T. ) ;
#19900 = CYLINDRICAL_SURFACE ( 'NONE', #4462, 2.844800000000001550 ) ;
#19901 = DIRECTION ( 'NONE',  ( 0.000000000000000000, 0.000000000000000000, -1.000000000000000000 ) ) ;
#19902 = ORIENTED_EDGE ( 'NONE', *, *, #15682, .T. ) ;
#19903 = DIRECTION ( 'NONE',  ( 7.280632624814000430E-13, -1.000000000000000000, 4.288485907146999317E-12 ) ) ;
#19904 = ORIENTED_EDGE ( 'NONE', *, *, #7505, .T. ) ;
#19905 = CARTESIAN_POINT ( 'NONE',  ( 10.36831320285999958, -3578.148799999999937, 2242.820000000000164 ) ) ;
#19906 = EDGE_CURVE ( 'NONE', #796, #21944, #22714, .T. ) ;
#19907 = DIRECTION ( 'NONE',  ( 1.000000000000000000, 0.000000000000000000, 0.000000000000000000 ) ) ;
#19908 = ORIENTED_EDGE ( 'NONE', *, *, #19582, .T. ) ;
#19909 = LINE ( 'NONE', #13439, #17403 ) ;
#19910 = CIRCLE ( 'NONE', #20638, 3.175000000000149925 ) ;
#19911 = AXIS2_PLACEMENT_3D ( 'NONE', #18034, #10771, #21556 ) ;
#19912 = ORIENTED_EDGE ( 'NONE', *, *, #8570, .T. ) ;
#19913 = CARTESIAN_POINT ( 'NONE',  ( 142.5942428639083062, -3695.644174312342329, 2254.886068105269260 ) ) ;
#19914 = DIRECTION ( 'NONE',  ( 0.000000000000000000, 0.000000000000000000, 1.000000000000000000 ) ) ;
#19915 = ORIENTED_EDGE ( 'NONE', *, *, #17525, .F. ) ;
#19916 = CARTESIAN_POINT ( 'NONE',  ( 137.5597807309948450, -3581.369168488304695, 2248.732576067342507 ) ) ;
#19917 = ORIENTED_EDGE ( 'NONE', *, *, #19156, .T. ) ;
#19918 = LINE ( 'NONE', #19690, #17477 ) ;
#19920 = AXIS2_PLACEMENT_3D ( 'NONE', #2087, #16599, #20681 ) ;
#19919 = APPROVAL_ROLE ( '' ) ;
#19921 = EDGE_CURVE ( 'NONE', #982, #16281, #2090, .T. ) ;
#19922 = DIRECTION ( 'NONE',  ( 0.000000000000000000, 0.000000000000000000, -1.000000000000000000 ) ) ;
#19923 = CARTESIAN_POINT ( 'NONE',  ( 8.088613972621001125, -3662.880847139000252, 2246.630000000000109 ) ) ;
#19924 = AXIS2_PLACEMENT_3D ( 'NONE', #21926, #14446, #12679 ) ;
#19925 = AXIS2_PLACEMENT_3D ( 'NONE', #8185, #12913, #6434 ) ;
#19926 = DIRECTION ( 'NONE',  ( 1.224646799147353207E-16, 1.000000000000000000, -0.000000000000000000 ) ) ;
#19927 = AXIS2_PLACEMENT_3D ( 'NONE', #16501, #15094, #14757 ) ;
#19928 = CARTESIAN_POINT ( 'NONE',  ( 138.3402197975327113, -3576.994575834084571, 2249.540499101924979 ) ) ;
#19929 = ORIENTED_EDGE ( 'NONE', *, *, #939, .T. ) ;
#19930 = CARTESIAN_POINT ( 'NONE',  ( 134.0716720153636743, -3578.501212890310853, 2244.568960851739121 ) ) ;
#19931 = VERTEX_POINT ( 'NONE', #6685 ) ;
#19932 = CARTESIAN_POINT ( 'NONE',  ( 137.1599999999999966, -3578.213872745999652, 2255.774000000000342 ) ) ;
#19933 = VERTEX_POINT ( 'NONE', #10296 ) ;
#19934 = CARTESIAN_POINT ( 'NONE',  ( 12.70000020906999971, -3582.339800010000090, 2257.592639999999847 ) ) ;
#19935 = CARTESIAN_POINT ( 'NONE',  ( 95.25000000000000000, -3568.700000000000273, 2247.392000000000280 ) ) ;
#19936 = AXIS2_PLACEMENT_3D ( 'NONE', #18557, #17022, #968 ) ;
#19937 = APPLIED_DATE_AND_TIME_ASSIGNMENT ( #6858, #21150, ( #20600 ) ) ;
#19938 = ORIENTED_EDGE ( 'NONE', *, *, #16012, .T. ) ;
#19939 = CARTESIAN_POINT ( 'NONE',  ( 10.36831320285999958, -3578.148799999999937, 2242.820000000000164 ) ) ;
#19940 = CYLINDRICAL_SURFACE ( 'NONE', #14802, 0.7619999999999294005 ) ;
#19941 = AXIS2_PLACEMENT_3D ( 'NONE', #14127, #15994, #23008 ) ;
#19942 = EDGE_LOOP ( 'NONE', ( #1272, #8451, #19123, #17822 ) ) ;
#19943 = VECTOR ( 'NONE', #4056, 1000.000000000000000 ) ;
#19944 = DIRECTION ( 'NONE',  ( 0.000000000000000000, 1.000000000000000000, 0.000000000000000000 ) ) ;
#19945 = PLANE ( 'NONE',  #22456 ) ;
#19946 = B_SPLINE_CURVE_WITH_KNOTS ( 'NONE', 3,
 ( #17559, #5160, #8559, #6914, #11830, #2926, #21091, #6691, #18985, #10066, #21214, #13594, #17209, #1156, #19443, #19216, #1508, #6451, #8319, #19097, #15464, #14058 ),
 .UNSPECIFIED., .F., .F.,
 ( 4, 2, 2, 1, 2, 2, 2, 1, 2, 2, 2, 4 ),
 ( 0.000000000000000000, 0.1250000000009205414, 0.1875000000011848578, 0.2187500000013189450, 0.2343750000014777624, 0.2500000000016365798, 0.3750000000026065816, 0.4375000000028015368, 0.4687500000027456371, 0.5000000000026897373, 0.7500000000013449242, 1.000000000000000000 ),
 .UNSPECIFIED. ) ;
#19947 = CARTESIAN_POINT ( 'NONE',  ( 12.70000000005999929, -3656.372659094999563, 2239.009999999999764 ) ) ;
#19948 = VERTEX_POINT ( 'NONE', #21084 ) ;
#19949 = CARTESIAN_POINT ( 'NONE',  ( 139.6999999999986528, -3662.197400000082780, 2239.391000000000076 ) ) ;
#19950 = APPROVAL_DATE_TIME ( #20292, #1322 ) ;
#19951 = ORIENTED_EDGE ( 'NONE', *, *, #16700, .T. ) ;
#19952 = AXIS2_PLACEMENT_3D ( 'NONE', #9891, #17160, #4289 ) ;
#19953 = DIRECTION ( 'NONE',  ( 0.000000000000000000, -2.331176954594000018E-14, -1.000000000000000000 ) ) ;
#19954 = FACE_OUTER_BOUND ( 'NONE', #2130, .T. ) ;
#19955 = EDGE_LOOP ( 'NONE', ( #12761, #7262, #19964, #7668 ) ) ;
#19956 = CARTESIAN_POINT ( 'NONE',  ( -12.70000000000007923, -3661.706170452909191, 2244.679313203225774 ) ) ;
#19957 = CARTESIAN_POINT ( 'NONE',  ( 137.7687556490391785, -3657.415903659005380, 2248.216200637740712 ) ) ;
#19958 = ORIENTED_EDGE ( 'NONE', *, *, #22461, .F. ) ;
#19959 = ORIENTED_EDGE ( 'NONE', *, *, #248, .T. ) ;
#19960 = VECTOR ( 'NONE', #22058, 1000.000000000000000 ) ;
#19961 = CARTESIAN_POINT ( 'NONE',  ( 137.4266760222526500, -3661.215795996489760, 2250.025794176416184 ) ) ;
#19962 = CLOSED_SHELL ( 'NONE', ( #1066, #10525, #19695, #9164, #17100, #5837, #6679, #15610, #12890, #3550, #18875, #21762, #10795, #13001, #12843, #21879, #15177, #16240, #16678, #9661 ) ) ;
#19963 = VERTEX_POINT ( 'NONE', #5154 ) ;
#19964 = ORIENTED_EDGE ( 'NONE', *, *, #22888, .T. ) ;
#19965 = ORIENTED_EDGE ( 'NONE', *, *, #11983, .F. ) ;
#19966 = PRODUCT_RELATED_PRODUCT_CATEGORY ( 'detail', '', ( #10108 ) ) ;
#19967 = CARTESIAN_POINT ( 'NONE',  ( 151.4000000000000057, -3694.938000000000102, 2296.591799999999694 ) ) ;
#19968 = ORIENTED_EDGE ( 'NONE', *, *, #4655, .F. ) ;
#19969 = ORIENTED_EDGE ( 'NONE', *, *, #829, .F. ) ;
#19970 = LINE ( 'NONE', #14467, #1924 ) ;
#19971 = CARTESIAN_POINT ( 'NONE',  ( 12.70000000003999929, -3662.197400000000016, 2242.820000000000164 ) ) ;
#19972 = VECTOR ( 'NONE', #8382, 1000.000000000000000 ) ;
#19973 = EDGE_LOOP ( 'NONE', ( #21269, #2875, #12126, #12660 ) ) ;
#19974 = LINE ( 'NONE', #5572, #14857 ) ;
#19975 = EDGE_CURVE ( 'NONE', #16187, #19707, #20963, .T. ) ;
#19976 = AXIS2_PLACEMENT_3D ( 'NONE', #8987, #18864, #2809 ) ;
#19977 = CARTESIAN_POINT ( 'NONE',  ( 7.231857318210721530, -3581.156156794382696, 2245.707491121732346 ) ) ;
#19978 = ADVANCED_FACE ( 'NONE', ( #12055 ), #19209, .T. ) ;
#19979 = CIRCLE ( 'NONE', #5715, 0.7619999999999294005 ) ;
#19980 = DIRECTION ( 'NONE',  ( 0.000000000000000000, -1.000000000000000000, 0.000000000000000000 ) ) ;
#19981 = CALENDAR_DATE ( 2026, 26, 10 ) ;
#19982 = EDGE_CURVE ( 'NONE', #11744, #10812, #12176, .T. ) ;
#19983 = AXIS2_PLACEMENT_3D ( 'NONE', #7507, #21584, #17824 ) ;
#19984 = CARTESIAN_POINT ( 'NONE',  ( -12.54218463262979988, -3658.793799999511066, 2249.723686797001392 ) ) ;
#19985 = EDGE_LOOP ( 'NONE', ( #8204, #10465, #2442, #9411 ) ) ;
#19986 = DIRECTION ( 'NONE',  ( 0.000000000000000000, 0.000000000000000000, -1.000000000000000000 ) ) ;
#19987 = EDGE_CURVE ( 'NONE', #22201, #19890, #15178, .T. ) ;
#19988 = ADVANCED_FACE ( 'NONE', ( #9356 ), #9468, .F. ) ;
#19989 = CARTESIAN_POINT ( 'NONE',  ( 12.69999999999999929, -3590.289999999999964, 2262.355140000000119 ) ) ;
#19990 = ORIENTED_EDGE ( 'NONE', *, *, #13883, .F. ) ;
#19991 = AXIS2_PLACEMENT_3D ( 'NONE', #22931, #19436, #14283 ) ;
#19992 = DIRECTION ( 'NONE',  ( -0.7249994335945012525, 0.000000000000000000, 0.6887494619146010688 ) ) ;
#19993 = CIRCLE ( 'NONE', #2753, 2.844799999999994444 ) ;
#19994 = ADVANCED_FACE ( 'NONE', ( #14634 ), #19792, .T. ) ;
#19995 = DIRECTION ( 'NONE',  ( 1.000000000000000000, 0.000000000000000000, 0.000000000000000000 ) ) ;
#19996 = DIRECTION ( 'NONE',  ( -0.000000000000000000, -1.000000000000000000, -0.000000000000000000 ) ) ;
#19997 = FACE_OUTER_BOUND ( 'NONE', #1843, .T. ) ;
#19998 = ORIENTED_EDGE ( 'NONE', *, *, #13807, .T. ) ;
#19999 = DIRECTION ( 'NONE',  ( 0.000000000000000000, 0.000000000000000000, -1.000000000000000000 ) ) ;
#20000 = ORIENTED_EDGE ( 'NONE', *, *, #19154, .F. ) ;
#20001 = CARTESIAN_POINT ( 'NONE',  ( 147.7813568978695002, -3695.700000000000728, 2259.444513961513167 ) ) ;
#20002 = CARTESIAN_POINT ( 'NONE',  ( 25.39999999999999858, -3578.860000000000127, 2247.392000000000280 ) ) ;
#20003 = CARTESIAN_POINT ( 'NONE',  ( 9.209369265563442042, -3543.299999999999727, 2282.113800000095125 ) ) ;
#20004 = CARTESIAN_POINT ( 'NONE',  ( 142.0316867971999955, -3578.148799999999937, 2242.820000000000164 ) ) ;
#20005 = CARTESIAN_POINT ( 'NONE',  ( 142.4126867973300534, -3577.928829547225178, 2239.009999999999764 ) ) ;
#20006 = AXIS2_PLACEMENT_3D ( 'NONE', #9822, #13347, #22237 ) ;
#20007 = CARTESIAN_POINT ( 'NONE',  ( 7.478703374698133288, -3577.171362236310415, 2245.102579701181639 ) ) ;
#20008 = VERTEX_POINT ( 'NONE', #7591 ) ;
#20009 = PERSON_AND_ORGANIZATION ( #5446, #1895 ) ;
#20010 = EDGE_CURVE ( 'NONE', #2058, #19085, #16493, .T. ) ;
#20011 = VECTOR ( 'NONE', #5356, 1000.000000000000000 ) ;
#20012 = CARTESIAN_POINT ( 'NONE',  ( 124.1552000000010025, -3568.700000000000273, 2259.837999999999738 ) ) ;
#20013 = DIRECTION ( 'NONE',  ( 0.000000000000000000, 0.000000000000000000, -1.000000000000000000 ) ) ;
#20014 = APPROVAL_ROLE ( '' ) ;
#20015 = ADVANCED_FACE ( 'NONE', ( #18365 ), #21777, .F. ) ;
#20016 = DIRECTION ( 'NONE',  ( 0.000000000000000000, 1.000000000000000000, 0.000000000000000000 ) ) ;
#20017 = EDGE_CURVE ( 'NONE', #22588, #20273, #11221, .T. ) ;
#20018 = PLANE ( 'NONE',  #5634 ) ;
#20019 = CARTESIAN_POINT ( 'NONE',  ( 15.54479999999999862, -3659.504999999999654, 2272.030000000000200 ) ) ;
#20020 = EDGE_LOOP ( 'NONE', ( #19584, #2419, #17678, #15405 ) ) ;
#20021 = FACE_OUTER_BOUND ( 'NONE', #22324, .T. ) ;
#20022 = ORIENTED_EDGE ( 'NONE', *, *, #19906, .T. ) ;
#20023 = AXIS2_PLACEMENT_3D ( 'NONE', #23024, #12138, #17521 ) ;
#20024 = FACE_OUTER_BOUND ( 'NONE', #17413, .T. ) ;
#20025 = AXIS2_PLACEMENT_3D ( 'NONE', #9214, #16355, #12492 ) ;
#20026 = CARTESIAN_POINT ( 'NONE',  ( 79.04479999999999507, -3568.700000000000273, 2261.869999999999891 ) ) ;
#20027 = EDGE_LOOP ( 'NONE', ( #5993, #4708, #13692, #4316 ) ) ;
#20028 = CARTESIAN_POINT ( 'NONE',  ( 54.40679999999999694, -3619.500000000000000, 2260.600000000000364 ) ) ;
#20029 = ADVANCED_FACE ( 'NONE', ( #16156 ), #11806, .T. ) ;
#20030 = ORIENTED_EDGE ( 'NONE', *, *, #15180, .T. ) ;
#20031 = CARTESIAN_POINT ( 'NONE',  ( 35.25520000000000209, -3594.099999999999909, 2261.869999999999891 ) ) ;
#20032 = DIRECTION ( 'NONE',  ( 0.000000000000000000, 0.000000000000000000, 1.000000000000000000 ) ) ;
#20033 = ORIENTED_EDGE ( 'NONE', *, *, #9378, .F. ) ;
#20034 = CARTESIAN_POINT ( 'NONE',  ( 137.7875023037999824, -3581.600928630999988, 2246.630000000000109 ) ) ;
#20035 = UNCERTAINTY_MEASURE_WITH_UNIT (LENGTH_MEASURE( 1.000000000000000082E-05 ), #19015, 'distance_accuracy_value', 'NONE');
#20036 = AXIS2_PLACEMENT_3D ( 'NONE', #19238, #6477, #3296 ) ;
#20037 = ORIENTED_EDGE ( 'NONE', *, *, #7721, .T. ) ;
#20038 = CARTESIAN_POINT ( 'NONE',  ( 145.4114788387173292, -3579.724573821726153, 2244.678944975163631 ) ) ;
#20039 = TOROIDAL_SURFACE ( 'NONE', #11045, 5.080000000000000071, 0.3810000000000000053 ) ;
#20040 = PERSON_AND_ORGANIZATION ( #5446, #1895 ) ;
#20041 = EDGE_CURVE ( 'NONE', #22749, #11737, #11117, .T. ) ;
#20042 = ADVANCED_FACE ( 'NONE', ( #14523 ), #7256, .F. ) ;
#20043 = VECTOR ( 'NONE', #23088, 1000.000000000000000 ) ;
#20044 = FACE_OUTER_BOUND ( 'NONE', #20911, .T. ) ;
#20045 = EDGE_CURVE ( 'NONE', #22687, #14575, #19681, .T. ) ;
#20046 = CARTESIAN_POINT ( 'NONE',  ( 139.6999999999999886, -3579.494999999999891, 2245.359999999999673 ) ) ;
#20047 = CARTESIAN_POINT ( 'NONE',  ( 132.0583097651000060, -3544.202533098000458, 2260.545675974999995 ) ) ;
#20048 = CARTESIAN_POINT ( 'NONE',  ( 11.88149704131999940, -3576.765771669000060, 2257.621751704000417 ) ) ;
#20049 = CARTESIAN_POINT ( 'NONE',  ( 141.4648100392906542, -3577.263639210850670, 2249.746746628647998 ) ) ;
#20050 = EDGE_CURVE ( 'NONE', #16669, #21367, #18480, .T. ) ;
#20051 = ORIENTED_EDGE ( 'NONE', *, *, #16247, .F. ) ;
#20052 = CARTESIAN_POINT ( 'NONE',  ( 134.4864491364314176, -3577.154038986648629, 2245.115470800847106 ) ) ;
#20053 = ORIENTED_EDGE ( 'NONE', *, *, #12439, .F. ) ;
#20054 = VECTOR ( 'NONE', #6077, 1000.000000000000000 ) ;
#20055 = CARTESIAN_POINT ( 'NONE',  ( 137.1599999999999966, -3658.223872745999870, 2255.774000000000342 ) ) ;
#20056 = CIRCLE ( 'NONE', #6572, 2.844799999999994444 ) ;
#20057 = EDGE_CURVE ( 'NONE', #15900, #8731, #8083, .T. ) ;
#20058 = EDGE_CURVE ( 'NONE', #424, #16601, #7478, .T. ) ;
#20059 = CIRCLE ( 'NONE', #23031, 5.460999999999938126 ) ;
#20060 = ORIENTED_EDGE ( 'NONE', *, *, #21618, .F. ) ;
#20061 = PLANE ( 'NONE',  #15040 ) ;
#20062 = CARTESIAN_POINT ( 'NONE',  ( 9.918918857905000053, -3598.871466521999537, 2279.464085466000142 ) ) ;
#20063 = VECTOR ( 'NONE', #1415, 1000.000000000000000 ) ;
#20064 = ORIENTED_EDGE ( 'NONE', *, *, #10815, .F. ) ;
#20065 = DIRECTION ( 'NONE',  ( 0.000000000000000000, -1.000000000000000000, 0.000000000000000000 ) ) ;
#20066 = CARTESIAN_POINT ( 'NONE',  ( 15.22954893437939283, -3578.192778017456476, 2250.157666245888777 ) ) ;
#20067 = SHAPE_REPRESENTATION_RELATIONSHIP ( 'NONE' , 'NONE' ,  #5332, #22185 ) ;
#20068 = PLANE ( 'NONE',  #22897 ) ;
#20069 = EDGE_LOOP ( 'NONE', ( #5681, #9772, #21271, #13657 ) ) ;
#20070 = CARTESIAN_POINT ( 'NONE',  ( 12.69997783158000004, -3636.657698770999559, 2279.817639764999967 ) ) ;
#20071 = CALENDAR_DATE ( 2026, 26, 10 ) ;
#20072 = DIRECTION ( 'NONE',  ( 0.000000000000000000, 0.000000000000000000, -1.000000000000000000 ) ) ;
#20073 = CARTESIAN_POINT ( 'NONE',  ( 151.1299999999999955, -3695.699999999999818, 2259.329999999999927 ) ) ;
#20074 = EDGE_LOOP ( 'NONE', ( #2522, #11989 ) ) ;
#20075 = DIRECTION ( 'NONE',  ( 2.330758767208999958E-14, 1.000000000000000000, 2.848874176402999842E-12 ) ) ;
#20076 = AXIS2_PLACEMENT_3D ( 'NONE', #14974, #6073, #13204 ) ;
#20077 = DIRECTION ( 'NONE',  ( 0.000000000000000000, 1.000000000000000000, 0.000000000000000000 ) ) ;
#20078 = AXIS2_PLACEMENT_3D ( 'NONE', #12046, #22926, #8652 ) ;
#20079 = VERTEX_POINT ( 'NONE', #22566 ) ;
#20080 = ORIENTED_EDGE ( 'NONE', *, *, #18562, .F. ) ;
#20081 = TOROIDAL_SURFACE ( 'NONE', #18556, 3.606799999999999784, 0.7620000000000000107 ) ;
#20082 = CARTESIAN_POINT ( 'NONE',  ( 137.8325232038615127, -3661.651965462245698, 2249.802177248667249 ) ) ;
#20083 = AXIS2_PLACEMENT_3D ( 'NONE', #3275, #1513, #4525 ) ;
#20084 = ORIENTED_EDGE ( 'NONE', *, *, #20262, .F. ) ;
#20085 = VERTEX_POINT ( 'NONE', #4527 ) ;
#20086 = LINE ( 'NONE', #390, #2069 ) ;
#20087 = ORIENTED_EDGE ( 'NONE', *, *, #13388, .F. ) ;
#20088 = CARTESIAN_POINT ( 'NONE',  ( 12.69999999999999929, -3639.502500000000055, 2288.971800000000258 ) ) ;
#20089 = CYLINDRICAL_SURFACE ( 'NONE', #7667, 2.844799999999994444 ) ;
#20090 = EDGE_LOOP ( 'NONE', ( #1264, #14689, #166, #18416 ) ) ;
#20091 = AXIS2_PLACEMENT_3D ( 'NONE', #10717, #21502, #17976 ) ;
#20092 = CARTESIAN_POINT ( 'NONE',  ( 136.6529205195000145, -3695.699999999999818, 2254.503999999999905 ) ) ;
#20093 = FACE_BOUND ( 'NONE', #16528, .T. ) ;
#20094 = CARTESIAN_POINT ( 'NONE',  ( 131.5729205195000020, -3543.299999999999727, 2259.329999999999927 ) ) ;
#20095 = CARTESIAN_POINT ( 'NONE',  ( 151.6380000000000052, -3694.938000000000102, 2296.591799999999694 ) ) ;
#20096 = AXIS2_PLACEMENT_3D ( 'NONE', #15634, #21368, #17365 ) ;
#20097 = APPROVAL_ROLE ( '' ) ;
#20098 = CARTESIAN_POINT ( 'NONE',  ( 20.32000000000000028, -3580.764999999999873, 2247.392000000000280 ) ) ;
#20099 = ORIENTED_EDGE ( 'NONE', *, *, #18454, .F. ) ;
#20100 = APPLIED_DATE_AND_TIME_ASSIGNMENT ( #32, #14564, ( #22796 ) ) ;
#20101 = CARTESIAN_POINT ( 'NONE',  ( 142.4930772826777456, -3658.963397008600623, 2249.982107089370857 ) ) ;
#20102 = EDGE_CURVE ( 'NONE', #5906, #18858, #884, .T. ) ;
#20103 = CARTESIAN_POINT ( 'NONE',  ( 7.107063980692033489, -3660.720702668381364, 2244.590566913373550 ) ) ;
#20104 = ORIENTED_EDGE ( 'NONE', *, *, #3219, .F. ) ;
#20105 = AXIS2_PLACEMENT_3D ( 'NONE', #21450, #16171, #16056 ) ;
#20106 = PLANE ( 'NONE',  #17056 ) ;
#20107 = AXIS2_PLACEMENT_3D ( 'NONE', #11512, #15273, #17015 ) ;
#20108 = ADVANCED_FACE ( 'NONE', ( #1121 ), #4338, .T. ) ;
#20109 = EDGE_CURVE ( 'NONE', #15378, #13988, #7939, .T. ) ;
#20110 = CARTESIAN_POINT ( 'NONE',  ( 12.69999999999999929, -3659.504999999999654, 2244.978999999999814 ) ) ;
#20111 = DIRECTION ( 'NONE',  ( 5.572969907074833723E-14, -1.000000000000000000, 0.000000000000000000 ) ) ;
#20112 = CARTESIAN_POINT ( 'NONE',  ( 139.6999999999999886, -3584.956000000000131, 2245.359999999999673 ) ) ;
#20114 = VERTEX_POINT ( 'NONE', #16725 ) ;
#20113 = EDGE_CURVE ( 'NONE', #2348, #8112, #17059, .T. ) ;
#20115 = CARTESIAN_POINT ( 'NONE',  ( 18.13064428604669942, -3657.724554382803944, 2245.888502604037512 ) ) ;
#20116 = VERTEX_POINT ( 'NONE', #16830 ) ;
#20117 = DIRECTION ( 'NONE',  ( 1.000000000000000000, 0.000000000000000000, 0.000000000000000000 ) ) ;
#20118 = DIRECTION ( 'NONE',  ( -1.206643234470999950E-12, 1.000000000000000000, 0.000000000000000000 ) ) ;
#20119 = CARTESIAN_POINT ( 'NONE',  ( 12.70000000003999929, -3662.197400000000016, 2239.391000000000076 ) ) ;
#20120 = CYLINDRICAL_SURFACE ( 'NONE', #17932, 2.844800000000091700 ) ;
#20121 = CARTESIAN_POINT ( 'NONE',  ( 142.7470794804999912, -3543.299999999999727, 2254.503999999999905 ) ) ;
#20122 = ADVANCED_FACE ( 'NONE', ( #6535 ), #8841, .T. ) ;
#20123 = CARTESIAN_POINT ( 'NONE',  ( 0.7620000000000000107, -3543.299999999999727, 2295.829799999999977 ) ) ;
#20124 = CARTESIAN_POINT ( 'NONE',  ( 7.114657506406928178, -3578.282732473625401, 2244.605386419569641 ) ) ;
#20125 = ORIENTED_EDGE ( 'NONE', *, *, #17425, .F. ) ;
#20126 = PERSON_AND_ORGANIZATION ( #5446, #1895 ) ;
#20127 = AXIS2_PLACEMENT_3D ( 'NONE', #8675, #15357, #17217 ) ;
#20128 = DIRECTION ( 'NONE',  ( 0.000000000000000000, -1.000000000000000000, 0.000000000000000000 ) ) ;
#20129 = LINE ( 'NONE', #16483, #14904 ) ;
#20130 = CIRCLE ( 'NONE', #14893, 2.844799999998998796 ) ;
#20131 = LINE ( 'NONE', #7580, #11308 ) ;
#20132 = VECTOR ( 'NONE', #2938, 1000.000000000000000 ) ;
#20133 = CARTESIAN_POINT ( 'NONE',  ( 12.70000000003999929, -3582.187399999999798, 2242.820000000000164 ) ) ;
#20134 = ORIENTED_EDGE ( 'NONE', *, *, #1625, .T. ) ;
#20135 = PLANE ( 'NONE',  #11883 ) ;
#20136 = ORIENTED_EDGE ( 'NONE', *, *, #10226, .F. ) ;
#20137 = DIRECTION ( 'NONE',  ( 0.000000000000000000, 1.000000000000000000, 0.000000000000000000 ) ) ;
#20138 = VERTEX_POINT ( 'NONE', #4308 ) ;
#20139 = EDGE_CURVE ( 'NONE', #2635, #15845, #9691, .T. ) ;
#20140 = DIRECTION ( 'NONE',  ( 0.000000000000000000, 0.000000000000000000, 1.000000000000000000 ) ) ;
#20141 = ADVANCED_FACE ( 'NONE', ( #15431 ), #9945, .T. ) ;
#20142 = AXIS2_PLACEMENT_3D ( 'NONE', #11006, #18150, #21787 ) ;
#20143 = DIRECTION ( 'NONE',  ( 0.000000000000000000, 1.000000000000000000, 0.000000000000000000 ) ) ;
#20144 = ORIENTED_EDGE ( 'NONE', *, *, #4933, .T. ) ;
#20145 = DIRECTION ( 'NONE',  ( -1.000000000000000000, 0.000000000000000000, 0.000000000000000000 ) ) ;
#20146 = DIRECTION ( 'NONE',  ( 0.000000000000000000, -1.000000000000000000, 0.000000000000000000 ) ) ;
#20147 = CIRCLE ( 'NONE', #6295, 2.844799999998998796 ) ;
#20148 = EDGE_LOOP ( 'NONE', ( #16594, #15459, #8844, #4395, #23116, #16874, #5894, #20282 ) ) ;
#20149 = DIRECTION ( 'NONE',  ( 2.324635735433000053E-14, 0.000000000000000000, 1.000000000000000000 ) ) ;
#20150 = DIRECTION ( 'NONE',  ( -1.000000000000000000, 0.000000000000000000, 0.000000000000000000 ) ) ;
#20151 = ORIENTED_EDGE ( 'NONE', *, *, #18401, .T. ) ;
#20152 = CARTESIAN_POINT ( 'NONE',  ( 12.69999999999999929, -3579.494999999999891, 2244.978999999999814 ) ) ;
#20153 = ORIENTED_EDGE ( 'NONE', *, *, #21334, .T. ) ;
#20154 = CARTESIAN_POINT ( 'NONE',  ( 145.3077377672685202, -3580.597427896025692, 2245.138331176687188 ) ) ;
#20155 = COORDINATED_UNIVERSAL_TIME_OFFSET ( 0, 0, .AHEAD. ) ;
#20156 = CARTESIAN_POINT ( 'NONE',  ( 145.3824765374318133, -3578.886079828094807, 2244.547288873628986 ) ) ;
#20157 = CARTESIAN_POINT ( 'NONE',  ( 18.28255762641966342, -3660.729247660008696, 2244.607872304181456 ) ) ;
#20158 = DIRECTION ( 'NONE',  ( 0.000000000000000000, 0.000000000000000000, -1.000000000000000000 ) ) ;
#20159 = DIRECTION ( 'NONE',  ( -1.000000000000000000, 0.000000000000000000, 0.000000000000000000 ) ) ;
#20160 = CARTESIAN_POINT ( 'NONE',  ( 138.9028968162981243, -3576.764073753475259, 2249.315552100089917 ) ) ;
#20161 = EDGE_LOOP ( 'NONE', ( #4448, #2544 ) ) ;
#20162 = CARTESIAN_POINT ( 'NONE',  ( 59.89320000000000022, -3594.099999999999909, 2239.009999999999764 ) ) ;
#20163 = ORIENTED_EDGE ( 'NONE', *, *, #7578, .T. ) ;
#20164 = PLANE ( 'NONE',  #23013 ) ;
#20165 = CARTESIAN_POINT ( 'NONE',  ( 142.5262129412070067, -3659.880018561507768, 2257.957971592014019 ) ) ;
#20166 = EDGE_CURVE ( 'NONE', #8549, #19050, #7696, .T. ) ;
#20167 = EDGE_CURVE ( 'NONE', #952, #16226, #676, .T. ) ;
#20168 = EDGE_LOOP ( 'NONE', ( #85, #744, #13894, #16955, #15640, #14643, #21940, #21778, #15841, #1986 ) ) ;
#20169 = EDGE_CURVE ( 'NONE', #1907, #21039, #20789, .T. ) ;
#20170 = PLANE ( 'NONE',  #21418 ) ;
#20171 = CARTESIAN_POINT ( 'NONE',  ( 15.49342176171425223, -3658.963902681101899, 2249.982338889249604 ) ) ;
#20172 = ORIENTED_EDGE ( 'NONE', *, *, #7106, .F. ) ;
#20173 = DIRECTION ( 'NONE',  ( 0.000000000000000000, 0.000000000000000000, 1.000000000000000000 ) ) ;
#20174 = CARTESIAN_POINT ( 'NONE',  ( 14.78006840248709608, -3577.552158459792736, 2249.919509794231089 ) ) ;
#20175 = CARTESIAN_POINT ( 'NONE',  ( 0.000000000000000000, 0.000000000000000000, 0.000000000000000000 ) ) ;
#20176 = DIRECTION ( 'NONE',  ( 0.6887494619146010688, 0.000000000000000000, -0.7249994335945012525 ) ) ;
#20177 = EDGE_CURVE ( 'NONE', #15879, #22049, #20821, .T. ) ;
#20178 = VERTEX_POINT ( 'NONE', #11556 ) ;
#20179 = LINE ( 'NONE', #13368, #12257 ) ;
#20180 = SECURITY_CLASSIFICATION_LEVEL ( 'unclassified' ) ;
#20181 = DIRECTION ( 'NONE',  ( 7.422379454680000104E-13, -1.000000000000000000, 4.288485907148999414E-12 ) ) ;
#20182 = CARTESIAN_POINT ( 'NONE',  ( 139.6999999999999886, -3579.494999999999891, 2239.391000000000076 ) ) ;
#20183 = VERTEX_POINT ( 'NONE', #2437 ) ;
#20184 = CARTESIAN_POINT ( 'NONE',  ( 18.13332411963230584, -3581.267160281976885, 2245.875868927712418 ) ) ;
#20185 = EDGE_CURVE ( 'NONE', #4963, #5042, #14455, .T. ) ;
#20186 = CARTESIAN_POINT ( 'NONE',  ( 151.1299999999999955, -3694.430000000000291, 2240.279999999999745 ) ) ;
#20187 = ADVANCED_FACE ( 'NONE', ( #22105 ), #12572, .T. ) ;
#20188 = EDGE_LOOP ( 'NONE', ( #12463, #17796 ) ) ;
#20189 = CIRCLE ( 'NONE', #19433, 0.7619999999999294005 ) ;
#20190 = CARTESIAN_POINT ( 'NONE',  ( 141.5845584249510978, -3661.638084686768707, 2249.811463398476462 ) ) ;
#20191 = EDGE_LOOP ( 'NONE', ( #17980, #21521, #9912, #20832, #17391, #22965 ) ) ;
#20192 = LINE ( 'NONE', #21941, #19220 ) ;
#20193 = EDGE_CURVE ( 'NONE', #19328, #9572, #6220, .T. ) ;
#20194 = CYLINDRICAL_SURFACE ( 'NONE', #2804, 2.844799999999009010 ) ;
#20195 = ORIENTED_EDGE ( 'NONE', *, *, #7303, .T. ) ;
#20196 = DIRECTION ( 'NONE',  ( 0.000000000000000000, 0.000000000000000000, -1.000000000000000000 ) ) ;
#20197 = PERSON_AND_ORGANIZATION ( #4596, #13896 ) ;
#20198 = CARTESIAN_POINT ( 'NONE',  ( -12.31899999999987116, -3578.860000000000127, 2252.853000000000065 ) ) ;
#20199 = CIRCLE ( 'NONE', #10077, 0.7619999999999294005 ) ;
#20200 = ORIENTED_EDGE ( 'NONE', *, *, #1102, .F. ) ;
#20201 = CARTESIAN_POINT ( 'NONE',  ( 12.69999999999999929, -3648.710000000000036, 2268.705139999999574 ) ) ;
#20202 = DIRECTION ( 'NONE',  ( 0.000000000000000000, 0.000000000000000000, -1.000000000000000000 ) ) ;
#20203 = CARTESIAN_POINT ( 'NONE',  ( 55.57575231171000496, -3695.699999999999818, 2275.763800000000174 ) ) ;
#20204 = LOCAL_TIME ( 17, 37, 43.00000000000000000, #22754 ) ;
#20205 = AXIS2_PLACEMENT_3D ( 'NONE', #22422, #15762, #4623 ) ;
#20206 = DIRECTION ( 'NONE',  ( 0.000000000000000000, 0.000000000000000000, -1.000000000000000000 ) ) ;
#20207 = COORDINATED_UNIVERSAL_TIME_OFFSET ( 0, 0, .AHEAD. ) ;
#20208 = CARTESIAN_POINT ( 'NONE',  ( 12.69997737251000025, -3602.342301254000176, 2279.817638609000369 ) ) ;
#20209 = ORIENTED_EDGE ( 'NONE', *, *, #6251, .F. ) ;
#20210 = CARTESIAN_POINT ( 'NONE',  ( 142.5172131144081789, -3659.103360921763397, 2250.042044413348322 ) ) ;
#20211 = PLANE ( 'NONE',  #665 ) ;
#20212 = EDGE_LOOP ( 'NONE', ( #21661, #18420, #20741, #15047 ) ) ;
#20213 = DIRECTION ( 'NONE',  ( 0.000000000000000000, -1.000000000000000000, 0.000000000000000000 ) ) ;
#20214 = AXIS2_PLACEMENT_3D ( 'NONE', #13112, #11010, #16745 ) ;
#20215 = LOCAL_TIME ( 17, 37, 43.00000000000000000, #12793 ) ;
#20216 = CARTESIAN_POINT ( 'NONE',  ( 127.0000000000000000, -3660.140000000000327, 2244.547199999999975 ) ) ;
#20217 = DIRECTION ( 'NONE',  ( -0.000000000000000000, -1.000000000000000000, -0.000000000000000000 ) ) ;
#20218 = DIRECTION ( 'NONE',  ( -1.000000000000000000, 0.000000000000000000, 0.000000000000000000 ) ) ;
#20219 = CARTESIAN_POINT ( 'NONE',  ( 12.69999999999999929, -3659.504999999999654, 2244.978999999999814 ) ) ;
#20220 = EDGE_LOOP ( 'NONE', ( #15242, #4846, #3500, #20084 ) ) ;
#20221 = CARTESIAN_POINT ( 'NONE',  ( 147.6115783649720186, -3695.579670240918858, 2259.869798073102174 ) ) ;
#20222 = CARTESIAN_POINT ( 'NONE',  ( 141.0563433985999779, -3577.145744321000166, 2239.391000000000076 ) ) ;
#20223 = CARTESIAN_POINT ( 'NONE',  ( 151.4000000000000057, -3543.299999999999727, 2280.589800000000196 ) ) ;
#20224 = APPLIED_PERSON_AND_ORGANIZATION_ASSIGNMENT ( #12421, #3625, ( #741 ) ) ;
#20225 = CARTESIAN_POINT ( 'NONE',  ( 101.5999999999999943, -3670.300000000000182, 2261.869999999999891 ) ) ;
#20226 = CARTESIAN_POINT ( 'NONE',  ( 7.619999999999999218, -3599.497499999999945, 2296.210799999999836 ) ) ;
#20227 = PLANE ( 'NONE',  #13203 ) ;
#20228 = DIRECTION ( 'NONE',  ( 0.000000000000000000, 1.000000000000000000, 0.000000000000000000 ) ) ;
#20229 = VERTEX_POINT ( 'NONE', #20576 ) ;
#20231 = AXIS2_PLACEMENT_3D ( 'NONE', #14166, #8768, #12398 ) ;
#20230 = APPROVAL_ROLE ( '' ) ;
#20232 = EDGE_CURVE ( 'NONE', #10874, #4775, #3969, .T. ) ;
#20233 = CARTESIAN_POINT ( 'NONE',  ( 92.50679999999999836, -3644.899999999999636, 2259.837999999999738 ) ) ;
#20234 = LOCAL_TIME ( 17, 37, 43.00000000000000000, #8908 ) ;
#20235 = LOCAL_TIME ( 17, 37, 43.00000000000000000, #14011 ) ;
#20236 = EDGE_CURVE ( 'NONE', #7405, #9937, #16946, .T. ) ;
#20237 = CARTESIAN_POINT ( 'NONE',  ( 139.6999999999999886, -3582.187399999999798, 2242.820000000000164 ) ) ;
#20238 = CARTESIAN_POINT ( 'NONE',  ( 104.4447999999999865, -3568.700000000000273, 2259.837999999999738 ) ) ;
#20239 = ORIENTED_EDGE ( 'NONE', *, *, #18815, .T. ) ;
#20240 = CARTESIAN_POINT ( 'NONE',  ( 134.8376892655312815, -3662.508216201634241, 2245.815664034198107 ) ) ;
#20241 = ORIENTED_EDGE ( 'NONE', *, *, #7015, .F. ) ;
#20242 = CARTESIAN_POINT ( 'NONE',  ( -5.588000000000000078, -3660.140000000000327, 2244.547199999999975 ) ) ;
#20243 = EDGE_LOOP ( 'NONE', ( #1042, #12715, #10636, #1282, #9627, #17259 ) ) ;
#20244 = CARTESIAN_POINT ( 'NONE',  ( 14.48593475403758468, -3661.719383861308415, 2249.758098224367586 ) ) ;
#20245 = CARTESIAN_POINT ( 'NONE',  ( 1.270000000000000018, -3660.140000000000327, 2250.236800000000130 ) ) ;
#20246 = VERTEX_POINT ( 'NONE', #6768 ) ;
#20247 = APPLIED_APPROVAL_ASSIGNMENT ( #16488, ( #3396 ) ) ;
#20248 = DIRECTION ( 'NONE',  ( 0.000000000000000000, -1.000000000000000000, 0.000000000000000000 ) ) ;
#20249 = PRODUCT_DEFINITION_FORMATION_WITH_SPECIFIED_SOURCE ( 'ANY', '', #12762, .NOT_KNOWN. ) ;
#20250 =( BOUNDED_CURVE ( )  B_SPLINE_CURVE ( 3, ( #19697, #21678, #19574, #14195 ),
 .UNSPECIFIED., .F., .T. ) 
 B_SPLINE_CURVE_WITH_KNOTS ( ( 4, 4 ),
 ( 1.570796326731764836, 3.141592653589793116 ),
 .UNSPECIFIED. ) 
 CURVE ( )  GEOMETRIC_REPRESENTATION_ITEM ( )  RATIONAL_B_SPLINE_CURVE ( ( 1.000000000000000000, 0.8047378541094847293, 0.8047378541094847293, 1.000000000000000000 ) ) 
 REPRESENTATION_ITEM ( '' )  );
#20251 = DIRECTION ( 'NONE',  ( 0.000000000000000000, -1.000000000000000000, 0.000000000000000000 ) ) ;
#20252 = APPLIED_PERSON_AND_ORGANIZATION_ASSIGNMENT ( #8618, #6640, ( #6775 ) ) ;
#20253 = ORIENTED_EDGE ( 'NONE', *, *, #18659, .F. ) ;
#20254 = FACE_OUTER_BOUND ( 'NONE', #20399, .T. ) ;
#20255 = DIRECTION ( 'NONE',  ( -1.000000000000000000, 0.000000000000000000, 0.000000000000000000 ) ) ;
#20256 = ORIENTED_EDGE ( 'NONE', *, *, #16681, .F. ) ;
#20257 = PRODUCT_DEFINITION_SHAPE ( 'NONE', 'NONE',  #23168 ) ;
#20258 = AXIS2_PLACEMENT_3D ( 'NONE', #21522, #17152, #13414 ) ;
#20259 = ADVANCED_FACE ( 'NONE', ( #16013 ), #5861, .T. ) ;
#20260 = CARTESIAN_POINT ( 'NONE',  ( 15.03168679716000078, -3658.158799999999701, 2242.820000000000164 ) ) ;
#20261 = UNCERTAINTY_MEASURE_WITH_UNIT (LENGTH_MEASURE( 1.000000000000000082E-05 ), #17013, 'distance_accuracy_value', 'NONE');
#20262 = EDGE_CURVE ( 'NONE', #22138, #19181, #12514, .T. ) ;
#20263 = ORIENTED_EDGE ( 'NONE', *, *, #12161, .F. ) ;
#20264 = LINE ( 'NONE', #9813, #13027 ) ;
#20265 = APPROVAL_DATE_TIME ( #4092, #18779 ) ;
#20266 = EDGE_CURVE ( 'NONE', #16784, #21023, #8086, .T. ) ;
#20267 = DIRECTION ( 'NONE',  ( 0.000000000000000000, 0.000000000000000000, -1.000000000000000000 ) ) ;
#20268 = FACE_OUTER_BOUND ( 'NONE', #9762, .T. ) ;
#20269 = CARTESIAN_POINT ( 'NONE',  ( 17.91090713674469015, -3661.851834046207841, 2245.119883787194794 ) ) ;
#20270 = FACE_OUTER_BOUND ( 'NONE', #15772, .T. ) ;
#20271 = CARTESIAN_POINT ( 'NONE',  ( 12.15081356636999921, -3576.699137309000434, 2257.605105499000274 ) ) ;
#20272 = CARTESIAN_POINT ( 'NONE',  ( 140.9034509249830194, -3576.915841627701411, 2249.469465256947387 ) ) ;
#20273 = VERTEX_POINT ( 'NONE', #10150 ) ;
#20274 = VECTOR ( 'NONE', #20805, 1000.000000000000000 ) ;
#20275 = TOROIDAL_SURFACE ( 'NONE', #5682, 3.606799999999999784, 0.7620000000000000107 ) ;
#20276 = FACE_OUTER_BOUND ( 'NONE', #20090, .T. ) ;
#20277 = EDGE_LOOP ( 'NONE', ( #17096, #11829 ) ) ;
#20278 = B_SPLINE_CURVE_WITH_KNOTS ( 'NONE', 3,
 ( #14117, #13999, #21030, #4848, #5324, #13769, #19617, #12000, #21149, #5094, #1328, #19386, #8495, #10593, #3320, #17501, #10472, #17617, #19498, #8725, #10709, #23000, #5211, #17856 ),
 .UNSPECIFIED., .F., .F.,
 ( 4, 2, 2, 1, 1, 1, 2, 2, 2, 2, 1, 2, 2, 4 ),
 ( 0.000000000000000000, 0.1250000000047984672, 0.1875000000071320172, 0.2187500000086201601, 0.2343750000093642316, 0.2421875000097362673, 0.2460937500095420061, 0.2500000000093477448, 0.3750000000084149354, 0.4375000000078757556, 0.4687500000073991369, 0.4843750000071607720, 0.5000000000069223516, 1.000000000000000000 ),
 .UNSPECIFIED. ) ;
#20279 = EDGE_CURVE ( 'NONE', #11877, #19707, #18934, .T. ) ;
#20280 = CARTESIAN_POINT ( 'NONE',  ( 10.89501796730999850, -3581.699918485000126, 2257.739459224999791 ) ) ;
#20281 = CYLINDRICAL_SURFACE ( 'NONE', #6512, 3.175000000000149925 ) ;
#20282 = ORIENTED_EDGE ( 'NONE', *, *, #2524, .T. ) ;
#20283 = DIRECTION ( 'NONE',  ( 0.000000000000000000, 0.000000000000000000, -1.000000000000000000 ) ) ;
#20284 = ORIENTED_EDGE ( 'NONE', *, *, #214, .F. ) ;
#20285 = CARTESIAN_POINT ( 'NONE',  ( 124.1552000000010025, -3619.500000000000000, 2261.869999999999891 ) ) ;
#20286 = CARTESIAN_POINT ( 'NONE',  ( 12.15970647189616116, -3576.701128706128202, 2249.244750392014794 ) ) ;
#20287 =( NAMED_UNIT ( * ) SI_UNIT ( $, .STERADIAN. ) SOLID_ANGLE_UNIT ( ) );
#20288 = CARTESIAN_POINT ( 'NONE',  ( 141.6584232981540765, -3581.559207404357039, 2248.295745760272894 ) ) ;
#20289 = EDGE_LOOP ( 'NONE', ( #9905, #9500, #7488, #7969 ) ) ;
#20291 = LINE ( 'NONE', #11374, #11491 ) ;
#20290 = CIRCLE ( 'NONE', #10173, 0.3809999999999647002 ) ;
#20292 = DATE_AND_TIME ( #20071, #9364 ) ;
#20293 = EDGE_CURVE ( 'NONE', #13309, #18286, #4877, .T. ) ;
#20294 = AXIS2_PLACEMENT_3D ( 'NONE', #12302, #1274, #20858 ) ;
#20295 = LINE ( 'NONE', #16771, #3270 ) ;
#20296 = CARTESIAN_POINT ( 'NONE',  ( 5.080000000000000071, -3694.430000000000291, 2260.600000000000364 ) ) ;
#20297 = VERTEX_POINT ( 'NONE', #6887 ) ;
#20298 = CARTESIAN_POINT ( 'NONE',  ( 20.66653435520565907, -3543.365340577194729, 2259.732141854306974 ) ) ;
#20299 = EDGE_CURVE ( 'NONE', #6734, #1484, #3238, .T. ) ;
#20300 = CARTESIAN_POINT ( 'NONE',  ( 139.5113177661436339, -3576.650200000001860, 2257.592639999999392 ) ) ;
#20301 = EDGE_CURVE ( 'NONE', #19931, #19068, #21058, .T. ) ;
#20302 = ORIENTED_EDGE ( 'NONE', *, *, #17147, .T. ) ;
#20303 = CIRCLE ( 'NONE', #17662, 2.844799999998995244 ) ;
#20304 = CARTESIAN_POINT ( 'NONE',  ( 15.54479999999999862, -3659.504999999999654, 2272.030000000000200 ) ) ;
#20305 = ORIENTED_EDGE ( 'NONE', *, *, #22408, .F. ) ;
#20306 = ORIENTED_EDGE ( 'NONE', *, *, #17954, .T. ) ;
#20307 = CIRCLE ( 'NONE', #21426, 5.460999999999938126 ) ;
#20308 = ORIENTED_EDGE ( 'NONE', *, *, #4675, .F. ) ;
#20309 = AXIS2_PLACEMENT_3D ( 'NONE', #19886, #5487, #5601 ) ;
#20310 = ORIENTED_EDGE ( 'NONE', *, *, #23119, .T. ) ;
#20311 = CARTESIAN_POINT ( 'NONE',  ( 20.82707948048999924, -3695.699999999999818, 2259.329999999999927 ) ) ;
#20312 = DIRECTION ( 'NONE',  ( -2.334777064352623371E-14, -1.000000000000000000, 0.000000000000000000 ) ) ;
#20313 = EDGE_CURVE ( 'NONE', #3892, #118, #12268, .T. ) ;
#20314 = EDGE_LOOP ( 'NONE', ( #5865, #16659, #8980 ) ) ;
#20315 = CIRCLE ( 'NONE', #22170, 3.606800000000021100 ) ;
#20316 = FACE_OUTER_BOUND ( 'NONE', #9085, .T. ) ;
#20317 =( LENGTH_UNIT ( ) NAMED_UNIT ( * ) SI_UNIT ( .MILLI., .METRE. ) );
#20318 = DIRECTION ( 'NONE',  ( 0.000000000000000000, 0.000000000000000000, 1.000000000000000000 ) ) ;
#20319 = DIRECTION ( 'NONE',  ( 0.000000000000000000, 0.000000000000000000, -1.000000000000000000 ) ) ;
#20320 = CIRCLE ( 'NONE', #12823, 2.844799999999994444 ) ;
#20321 = APPROVAL_DATE_TIME ( #13397, #13489 ) ;
#20322 = CARTESIAN_POINT ( 'NONE',  ( 151.4000000000000057, -3660.140000000000327, 2250.265832635400784 ) ) ;
#20323 = EDGE_LOOP ( 'NONE', ( #3377, #6478, #15288, #16726 ) ) ;
#20324 = AXIS2_PLACEMENT_3D ( 'NONE', #15323, #11672, #19066 ) ;
#20325 = AXIS2_PLACEMENT_3D ( 'NONE', #21869, #13075, #9673 ) ;
#20326 = DIRECTION ( 'NONE',  ( -1.000000000000000000, 0.000000000000000000, 0.000000000000000000 ) ) ;
#20327 = ADVANCED_FACE ( 'NONE', ( #10502 ), #3118, .T. ) ;
#20328 = DIRECTION ( 'NONE',  ( 0.000000000000000000, 0.000000000000000000, 1.000000000000000000 ) ) ;
#20329 = EDGE_LOOP ( 'NONE', ( #16975, #19761, #12251, #13383 ) ) ;
#20330 = DIRECTION ( 'NONE',  ( 0.000000000000000000, 0.000000000000000000, 1.000000000000000000 ) ) ;
#20331 = FACE_OUTER_BOUND ( 'NONE', #13789, .T. ) ;
#20332 = ORIENTED_EDGE ( 'NONE', *, *, #15553, .F. ) ;
#20333 = CIRCLE ( 'NONE', #7989, 0.7619999999999294005 ) ;
#20334 = ORIENTED_EDGE ( 'NONE', *, *, #6126, .F. ) ;
#20335 = DIRECTION ( 'NONE',  ( 0.000000000000000000, -1.000000000000000000, 0.000000000000000000 ) ) ;
#20336 = EDGE_LOOP ( 'NONE', ( #264, #14326 ) ) ;
#20337 = ORIENTED_EDGE ( 'NONE', *, *, #21107, .T. ) ;
#20338 = LINE ( 'NONE', #1210, #6044 ) ;
#20339 = DIRECTION ( 'NONE',  ( -0.7071067811864976127, 0.000000000000000000, 0.7071067811865975328 ) ) ;
#20340 = AXIS2_PLACEMENT_3D ( 'NONE', #1218, #1454, #10129 ) ;
#20341 = DIRECTION ( 'NONE',  ( -1.000000000000000000, 0.000000000000000000, 2.324635735433000053E-14 ) ) ;
#20342 = EDGE_CURVE ( 'NONE', #14706, #6665, #22865, .T. ) ;
#20343 = DIRECTION ( 'NONE',  ( 0.000000000000000000, 0.000000000000000000, -1.000000000000000000 ) ) ;
#20344 = FACE_OUTER_BOUND ( 'NONE', #8558, .T. ) ;
#20345 = CARTESIAN_POINT ( 'NONE',  ( 64.76999999999999602, -3543.299999999999727, 2289.213099999999940 ) ) ;
#20346 = ORIENTED_EDGE ( 'NONE', *, *, #15846, .F. ) ;
#20347 = COORDINATED_UNIVERSAL_TIME_OFFSET ( 0, 0, .AHEAD. ) ;
#20348 = CARTESIAN_POINT ( 'NONE',  ( -12.31900000000000084, -3661.486200000000281, 2245.060313203000078 ) ) ;
#20349 = CIRCLE ( 'NONE', #9490, 5.460999999999938126 ) ;
#20350 = DIRECTION ( 'NONE',  ( 0.000000000000000000, 0.000000000000000000, -1.000000000000000000 ) ) ;
#20351 = CARTESIAN_POINT ( 'NONE',  ( 15.03168679714000078, -3638.156300000000101, 2292.781800000000203 ) ) ;
#20352 = ORIENTED_EDGE ( 'NONE', *, *, #13148, .F. ) ;
#20353 = CARTESIAN_POINT ( 'NONE',  ( 134.8815275705442502, -3662.578409907537662, 2245.925647646461130 ) ) ;
#20354 = CARTESIAN_POINT ( 'NONE',  ( 139.6999999999999886, -3579.494999999999891, 2246.630000000000109 ) ) ;
#20355 = VERTEX_POINT ( 'NONE', #14259 ) ;
#20356 = CARTESIAN_POINT ( 'NONE',  ( 54.40679999999999694, -3568.700000000000273, 2239.009999999999764 ) ) ;
#20357 = CARTESIAN_POINT ( 'NONE',  ( 13.23165581431225846, -3662.300617105160200, 2249.242775709399211 ) ) ;
#20358 = DIRECTION ( 'NONE',  ( 0.000000000000000000, 0.000000000000000000, 1.000000000000000000 ) ) ;
#20359 = VERTEX_POINT ( 'NONE', #22792 ) ;
#20360 = CARTESIAN_POINT ( 'NONE',  ( 6.985000000000000320, -3639.502500000000055, 2288.971800000000258 ) ) ;
#20361 = DIRECTION ( 'NONE',  ( 1.000000000000000000, 0.000000000000000000, 0.000000000000000000 ) ) ;
#20362 = LINE ( 'NONE', #6193, #3700 ) ;
#20363 = CARTESIAN_POINT ( 'NONE',  ( 63.50000000000000000, -3644.899999999999636, 2261.869999999999891 ) ) ;
#20364 = EDGE_LOOP ( 'NONE', ( #5247, #11585, #4888, #21122 ) ) ;
#20365 = ORIENTED_EDGE ( 'NONE', *, *, #6945, .T. ) ;
#20366 = CARTESIAN_POINT ( 'NONE',  ( 137.3683132028983493, -3658.158799999801431, 2239.167815367335152 ) ) ;
#20367 = VERTEX_POINT ( 'NONE', #8753 ) ;
#20368 = CARTESIAN_POINT ( 'NONE',  ( 16.19063073439513190, -3543.299999999999727, 2282.113800000000083 ) ) ;
#20369 = APPROVAL_DATE_TIME ( #3860, #13928 ) ;
#20370 = CARTESIAN_POINT ( 'NONE',  ( 3.810000000000000053, -3694.938000000000102, 2229.612000000000080 ) ) ;
#20371 = CARTESIAN_POINT ( 'NONE',  ( 17.91260410565400463, -3661.848063305847063, 2245.117046218366340 ) ) ;
#20372 = AXIS2_PLACEMENT_3D ( 'NONE', #10844, #19635, #19873 ) ;
#20373 = DIRECTION ( 'NONE',  ( -1.000000000000000000, 0.000000000000000000, 0.000000000000000000 ) ) ;
#20374 = APPLIED_PERSON_AND_ORGANIZATION_ASSIGNMENT ( #1076, #21130, ( #11230 ) ) ;
#20375 = TOROIDAL_SURFACE ( 'NONE', #180, 3.606799999999999784, 0.7620000000000000107 ) ;
#20376 = CARTESIAN_POINT ( 'NONE',  ( 10.68485228337000059, -3577.480333023000185, 2257.776247070999943 ) ) ;
#20377 = DIRECTION ( 'NONE',  ( -0.7249994335945011414, 0.000000000000000000, -0.6887494619146010688 ) ) ;
#20378 = ORIENTED_EDGE ( 'NONE', *, *, #6540, .T. ) ;
#20379 = CARTESIAN_POINT ( 'NONE',  ( 7.363939561626733799, -3657.457649646252776, 2246.419592195776659 ) ) ;
#20380 = EDGE_CURVE ( 'NONE', #7706, #4416, #4696, .T. ) ;
#20381 = CARTESIAN_POINT ( 'NONE',  ( 35.56000000000000227, -3544.570000000000164, 2243.277199999999993 ) ) ;
#20382 = ORIENTED_EDGE ( 'NONE', *, *, #19841, .F. ) ;
#20383 = EDGE_CURVE ( 'NONE', #21944, #17042, #5594, .T. ) ;
#20384 = DIRECTION ( 'NONE',  ( 0.000000000000000000, 0.000000000000000000, -1.000000000000000000 ) ) ;
#20385 = CARTESIAN_POINT ( 'NONE',  ( 140.4385240681895084, -3662.258542810513973, 2257.615706727033739 ) ) ;
#20386 = ADVANCED_FACE ( 'NONE', ( #18109 ), #21637, .F. ) ;
#20387 = ORIENTED_EDGE ( 'NONE', *, *, #6832, .F. ) ;
#20388 = ORIENTED_EDGE ( 'NONE', *, *, #742, .T. ) ;
#20389 = DIRECTION ( 'NONE',  ( 0.000000000000000000, 0.000000000000000000, 1.000000000000000000 ) ) ;
#20390 = AXIS2_PLACEMENT_3D ( 'NONE', #11413, #20544, #18570 ) ;
#20391 = AXIS2_PLACEMENT_3D ( 'NONE', #8340, #18335, #7670 ) ;
#20392 = ORIENTED_EDGE ( 'NONE', *, *, #19843, .F. ) ;
#20393 = CIRCLE ( 'NONE', #929, 2.873832635400752622 ) ;
#20394 = CARTESIAN_POINT ( 'NONE',  ( 0.7620000000000000107, -3543.299999999999727, 2275.763800000000174 ) ) ;
#20395 = CARTESIAN_POINT ( 'NONE',  ( 15.39520459006179287, -3578.572279200602679, 2250.225720840873237 ) ) ;
#20396 = AXIS2_PLACEMENT_3D ( 'NONE', #18060, #19714, #263 ) ;
#20397 = EDGE_CURVE ( 'NONE', #946, #7196, #12840, .T. ) ;
#20398 = CARTESIAN_POINT ( 'NONE',  ( 142.0826489325229147, -3581.049212494424410, 2249.208663835029711 ) ) ;
#20399 = EDGE_LOOP ( 'NONE', ( #22971, #16249, #3878, #16915, #7902, #12879 ) ) ;
#20400 = CARTESIAN_POINT ( 'NONE',  ( 151.1299999999999955, -3694.430000000000291, 2240.279999999999745 ) ) ;
#20401 = CALENDAR_DATE ( 2026, 26, 10 ) ;
#20402 = CARTESIAN_POINT ( 'NONE',  ( 139.6999999997612747, -3662.637340905137989, 2239.009999999999764 ) ) ;
#20403 = CARTESIAN_POINT ( 'NONE',  ( 151.4000000000000057, -3695.699999999999818, 2280.589800000000196 ) ) ;
#20404 = EDGE_CURVE ( 'NONE', #8967, #14295, #14608, .T. ) ;
#20405 = CARTESIAN_POINT ( 'NONE',  ( 137.2160574923763079, -3578.059772265523407, 2257.872821569613279 ) ) ;
#20406 = AXIS2_PLACEMENT_3D ( 'NONE', #10443, #15839, #22970 ) ;
#20407 = EDGE_LOOP ( 'NONE', ( #3475, #14528, #4766, #12258 ) ) ;
#20408 = TOROIDAL_SURFACE ( 'NONE', #8069, 4.114799999999999791, 1.270000000000000018 ) ;
#20409 = DIRECTION ( 'NONE',  ( 0.000000000000000000, 0.000000000000000000, -1.000000000000000000 ) ) ;
#20410 = CIRCLE ( 'NONE', #6574, 4.114799999999974034 ) ;
#20411 = EDGE_LOOP ( 'NONE', ( #22592, #9617, #17704, #9687 ) ) ;
#20412 = ORIENTED_EDGE ( 'NONE', *, *, #16807, .F. ) ;
#20413 = EDGE_LOOP ( 'NONE', ( #2942, #5512, #13427, #21835 ) ) ;
#20414 = ADVANCED_FACE ( 'NONE', ( #5475 ), #5706, .F. ) ;
#20415 = ADVANCED_FACE ( 'NONE', ( #11087 ), #21934, .T. ) ;
#20416 = CARTESIAN_POINT ( 'NONE',  ( 15.41268679713999923, -3639.502500000000055, 2296.210799999999836 ) ) ;
#20417 = ORIENTED_EDGE ( 'NONE', *, *, #14971, .F. ) ;
#20418 = LINE ( 'NONE', #623, #21013 ) ;
#20419 = CARTESIAN_POINT ( 'NONE',  ( 9.987313202864001482, -3581.061170452999704, 2239.009999999999764 ) ) ;
#20420 = EDGE_LOOP ( 'NONE', ( #7932, #3678, #6222, #9380 ) ) ;
#20421 = LINE ( 'NONE', #20527, #9967 ) ;
#20422 = DIRECTION ( 'NONE',  ( 0.000000000000000000, -1.000000000000000000, 0.000000000000000000 ) ) ;
#20423 = DIRECTION ( 'NONE',  ( 0.000000000000000000, 0.000000000000000000, 1.000000000000000000 ) ) ;
#20424 = CIRCLE ( 'NONE', #11059, 0.7619999999999996776 ) ;
#20425 = AXIS2_PLACEMENT_3D ( 'NONE', #16385, #5962, #14402 ) ;
#20426 = DIRECTION ( 'NONE',  ( -1.122008997397786234E-13, 0.000000000000000000, -1.000000000000000000 ) ) ;
#20427 = APPROVAL_STATUS ( 'not_yet_approved' ) ;
#20428 = AXIS2_PLACEMENT_3D ( 'NONE', #6436, #15684, #20956 ) ;
#20429 = DIRECTION ( 'NONE',  ( 1.000000000000000000, 0.000000000000000000, 0.000000000000000000 ) ) ;
#20430 = VERTEX_POINT ( 'NONE', #21969 ) ;
#20431 = CARTESIAN_POINT ( 'NONE',  ( 12.69999999999999929, -3639.502500000000055, 2263.571799999999712 ) ) ;
#20432 = DIRECTION ( 'NONE',  ( 0.000000000000000000, 0.000000000000000000, -1.000000000000000000 ) ) ;
#20433 = VECTOR ( 'NONE', #20735, 1000.000000000000000 ) ;
#20434 = ORIENTED_EDGE ( 'NONE', *, *, #13874, .T. ) ;
#20435 = CARTESIAN_POINT ( 'NONE',  ( 137.0453141145324309, -3543.765301131294109, 2255.486744313127929 ) ) ;
#20436 = VECTOR ( 'NONE', #19273, 1000.000000000000000 ) ;
#20437 = CARTESIAN_POINT ( 'NONE',  ( 139.6999999999999886, -3659.504999999999654, 2245.359999999999673 ) ) ;
#20438 = B_SPLINE_CURVE_WITH_KNOTS ( 'NONE', 3,
 ( #19718, #20506, #20395, #13131, #9729, #20066, #2246, #14906, #16530, #9396, #18293, #13243, #15014, #6230, #7865, #9840, #2478, #20174, #7981, #18407, #600, #16643, #13029, #18521, #22033, #9620, #22144, #21925, #16766, #2363, #6344, #2582, #485, #7625, #7754, #5997, #5892, #814, #11486, #6117, #18636, #14786, #20286, #4114, #11259, #9502, #4347, #16871, #13364, #15126, #16984, #711, #4232, #22255, #11369, #4454, #11592, #18743, #2692, #931, #8099, #15244, #22371, #4004, #11152, #1842, #7017, #6457, #20862, #17773, #3474, #12390, #15471, #11711, #19423, #21416, #14159, #19534 ),
 .UNSPECIFIED., .F., .F.,
 ( 4, 2, 2, 1, 2, 2, 2, 1, 2, 2, 2, 1, 2, 2, 2, 2, 2, 2, 1, 2, 2, 2, 2, 2, 1, 2, 2, 2, 2, 2, 2, 1, 2, 2, 2, 1, 2, 2, 2, 1, 2, 2, 4 ),
 ( 0.000000000000000000, 0.06249999999819785823, 0.09374999999739346002, 0.1093749999970090869, 0.1171874999969127751, 0.1249999999968164632, 0.1562499999965751007, 0.1718749999963936348, 0.1796874999963606334, 0.1874999999963276320, 0.2187499999966426856, 0.2343749999967737474, 0.2421874999968235131, 0.2499999999968732789, 0.2812499999972781217, 0.2968749999974463205, 0.3124999999976144638, 0.3437499999978942400, 0.3593749999980610510, 0.3671874999981183940, 0.3749999999981757370, 0.4999999999991848743, 0.5624999999996890265, 0.5937499999999581446, 0.6093750000000727196, 0.6171875000001783018, 0.6250000000002837730, 0.6562500000007047696, 0.6718750000008879564, 0.6875000000010711432, 0.7187500000014369617, 0.7343750000015929480, 0.7421875000016709967, 0.7500000000017490454, 0.7812500000019865221, 0.7968750000020596858, 0.8046875000020707880, 0.8125000000020818902, 0.8437500000016395774, 0.8593750000013337109, 0.8671875000012222445, 0.8750000000011106671, 1.000000000000000000 ),
 .UNSPECIFIED. ) ;
#20439 = EDGE_LOOP ( 'NONE', ( #11175, #405, #17101, #18301 ) ) ;
#20440 = CARTESIAN_POINT ( 'NONE',  ( 140.4385240661417527, -3582.248542811027164, 2257.615706726905501 ) ) ;
#20441 = PRODUCT_DEFINITION_SHAPE ( 'NONE', 'NONE',  #22928 ) ;
#20442 = AXIS2_PLACEMENT_3D ( 'NONE', #10830, #171, #21620 ) ;
#20443 = DIRECTION ( 'NONE',  ( -1.000000000000000000, -1.165588477296754225E-12, 0.000000000000000000 ) ) ;
#20444 = EDGE_LOOP ( 'NONE', ( #15120, #14383, #4248, #3387 ) ) ;
#20445 = ORIENTED_EDGE ( 'NONE', *, *, #4975, .F. ) ;
#20446 = DIRECTION ( 'NONE',  ( 1.000000000000000000, 0.000000000000000000, 0.000000000000000000 ) ) ;
#20447 = CARTESIAN_POINT ( 'NONE',  ( 20.25432815367999950, -3694.678775005999796, 2260.506484774000000 ) ) ;
#20448 = SHAPE_REPRESENTATION ( 'MAT-035', ( #6777, #8609, #21342, #4869, #4124, #18711, #8992, #7125, #8624, #21711, #10101, #7874, #14, #13106, #2994, #6009 ), #4887 ) ;
#20449 = CARTESIAN_POINT ( 'NONE',  ( 11.76763247656000111, -3602.191447740999592, 2279.779831143999672 ) ) ;
#20450 = ADVANCED_FACE ( 'NONE', ( #7562 ), #12725, .F. ) ;
#20451 = EDGE_CURVE ( 'NONE', #16435, #16187, #13665, .T. ) ;
#20452 = AXIS2_PLACEMENT_3D ( 'NONE', #13668, #15315, #20818 ) ;
#20453 = CARTESIAN_POINT ( 'NONE',  ( 22.54063073453000143, -3694.938000000000102, 2275.001800000000003 ) ) ;
#20454 = CARTESIAN_POINT ( 'NONE',  ( 15.03168679716000078, -3658.158799999999701, 2242.820000000000164 ) ) ;
#20455 = ADVANCED_FACE ( 'NONE', ( #9549 ), #4393, .T. ) ;
#20456 = CARTESIAN_POINT ( 'NONE',  ( 7.953724235889067629, -3576.303814212001726, 2246.097598271465813 ) ) ;
#20457 = VERTEX_POINT ( 'NONE', #980 ) ;
#20458 = CALENDAR_DATE ( 2026, 26, 10 ) ;
#20459 = DIRECTION ( 'NONE',  ( 0.000000000000000000, 0.000000000000000000, -1.000000000000000000 ) ) ;
#20460 = EDGE_CURVE ( 'NONE', #20823, #424, #3581, .T. ) ;
#20461 = DIRECTION ( 'NONE',  ( 0.000000000000000000, 0.000000000000000000, -1.000000000000000000 ) ) ;
#20462 = AXIS2_PLACEMENT_3D ( 'NONE', #18773, #2719, #15044 ) ;
#20463 = DIRECTION ( 'NONE',  ( -1.000000000000000000, 0.000000000000000000, 0.000000000000000000 ) ) ;
#20464 = VERTEX_POINT ( 'NONE', #2735 ) ;
#20465 = EDGE_CURVE ( 'NONE', #473, #10571, #21578, .T. ) ;
#20466 = LINE ( 'NONE', #9788, #14459 ) ;
#20467 = ORIENTED_EDGE ( 'NONE', *, *, #13290, .F. ) ;
#20468 = EDGE_CURVE ( 'NONE', #2777, #18533, #13522, .T. ) ;
#20469 = DIRECTION ( 'NONE',  ( 1.000000000000000000, 0.000000000000000000, 6.993530863773999741E-14 ) ) ;
#20470 = CARTESIAN_POINT ( 'NONE',  ( 134.6160622235418884, -3576.882542126288627, 2245.342794667374164 ) ) ;
#20471 = ORIENTED_EDGE ( 'NONE', *, *, #22986, .F. ) ;
#20472 = CARTESIAN_POINT ( 'NONE',  ( 5.080000000000000071, -3544.570000000000164, 2260.600000000000364 ) ) ;
#20473 = DIRECTION ( 'NONE',  ( 0.000000000000000000, 0.000000000000000000, -1.000000000000000000 ) ) ;
#20474 = DIRECTION ( 'NONE',  ( 0.000000000000000000, 0.000000000000000000, -1.000000000000000000 ) ) ;
#20475 = ORIENTED_EDGE ( 'NONE', *, *, #9859, .F. ) ;
#20476 = CARTESIAN_POINT ( 'NONE',  ( 22.00181536726000076, -3694.938000000000102, 2275.224984633000076 ) ) ;
#20477 = DIRECTION ( 'NONE',  ( -1.000000000000000000, 0.000000000000000000, 0.000000000000000000 ) ) ;
#20478 = CARTESIAN_POINT ( 'NONE',  ( 136.8552000000009912, -3579.494999999999891, 2257.962944264955695 ) ) ;
#20479 = CARTESIAN_POINT ( 'NONE',  ( 12.69999999999999929, -3649.471999999999753, 2268.705139999999574 ) ) ;
#20480 = ORIENTED_EDGE ( 'NONE', *, *, #21182, .T. ) ;
#20481 = ORIENTED_EDGE ( 'NONE', *, *, #15467, .F. ) ;
#20482 = CIRCLE ( 'NONE', #2166, 0.7619999999999294005 ) ;
#20483 = CIRCLE ( 'NONE', #14143, 5.460999999999938126 ) ;
#20484 = CYLINDRICAL_SURFACE ( 'NONE', #13930, 2.844799999999999773 ) ;
#20485 = AXIS2_PLACEMENT_3D ( 'NONE', #10068, #19448, #14063 ) ;
#20486 = ORIENTED_EDGE ( 'NONE', *, *, #15049, .T. ) ;
#20487 = CARTESIAN_POINT ( 'NONE',  ( -12.31900000000000084, -3576.510744320999947, 2248.748343399000532 ) ) ;
#20488 = CARTESIAN_POINT ( 'NONE',  ( 140.6228164711258728, -3576.797677065675089, 2257.629692243157024 ) ) ;
#20489 = CARTESIAN_POINT ( 'NONE',  ( 17.91462652069883177, -3661.843557398242410, 2245.113670094950066 ) ) ;
#20490 = DIRECTION ( 'NONE',  ( -1.000000000000000000, 0.000000000000000000, 0.000000000000000000 ) ) ;
#20491 = DIRECTION ( 'NONE',  ( -2.334777064352623371E-14, -1.000000000000000000, 0.000000000000000000 ) ) ;
#20492 = AXIS2_PLACEMENT_3D ( 'NONE', #20647, #20013, #8133 ) ;
#20493 = DIRECTION ( 'NONE',  ( -1.000000000000000000, -5.378139827789999268E-13, 1.344534956946999995E-13 ) ) ;
#20494 = ORIENTED_EDGE ( 'NONE', *, *, #10143, .F. ) ;
#20495 = CYLINDRICAL_SURFACE ( 'NONE', #5849, 2.844799999999999773 ) ;
#20496 = FACE_OUTER_BOUND ( 'NONE', #17621, .T. ) ;
#20497 = ORIENTED_EDGE ( 'NONE', *, *, #3399, .T. ) ;
#20498 = DIRECTION ( 'NONE',  ( 0.000000000000000000, 0.000000000000000000, -1.000000000000000000 ) ) ;
#20499 = CARTESIAN_POINT ( 'NONE',  ( 140.9635494355036940, -3662.060586539072119, 2257.663356974682301 ) ) ;
#20500 = VERTEX_POINT ( 'NONE', #4615 ) ;
#20501 = ORIENTED_EDGE ( 'NONE', *, *, #13995, .F. ) ;
#20502 = EDGE_LOOP ( 'NONE', ( #21834, #4280, #20560, #22019 ) ) ;
#20503 = PRODUCT_DEFINITION ( 'UNKNOWN', '', #3730, #4563 ) ;
#20504 = VECTOR ( 'NONE', #13864, 1000.000000000000000 ) ;
#20505 = CARTESIAN_POINT ( 'NONE',  ( 142.2400000000000091, -3658.223872745999870, 2255.774000000000342 ) ) ;
#20506 = CARTESIAN_POINT ( 'NONE',  ( 15.43982607913381244, -3578.715157675396313, 2250.236799999999675 ) ) ;
#20507 = DIRECTION ( 'NONE',  ( 1.000000000000000000, 0.000000000000000000, 0.000000000000000000 ) ) ;
#20508 = CARTESIAN_POINT ( 'NONE',  ( 142.5448000000000093, -3579.687792440064641, 2250.120875928858368 ) ) ;
#20509 = ORIENTED_EDGE ( 'NONE', *, *, #1771, .F. ) ;
#20510 = CARTESIAN_POINT ( 'NONE',  ( 137.1599999999999966, -3580.776127254000130, 2255.774000000000342 ) ) ;
#20511 = DATE_AND_TIME ( #4574, #16820 ) ;
#20512 = ADVANCED_FACE ( 'NONE', ( #11754 ), #10006, .T. ) ;
#20513 = CARTESIAN_POINT ( 'NONE',  ( 139.6999999999999886, -3582.187399999999798, 2242.820000000000164 ) ) ;
#20514 = CARTESIAN_POINT ( 'NONE',  ( 20.68110872146951351, -3543.353673605964104, 2259.695705217817704 ) ) ;
#20515 = EDGE_CURVE ( 'NONE', #21382, #22597, #15171, .T. ) ;
#20516 = CARTESIAN_POINT ( 'NONE',  ( -12.70000000000005080, -3663.272340905245528, 2247.392000000001644 ) ) ;
#20517 = EDGE_LOOP ( 'NONE', ( #19738, #7950, #11715, #15018, #9697, #8575 ) ) ;
#20518 = PLANE ( 'NONE',  #13305 ) ;
#20519 = ORIENTED_EDGE ( 'NONE', *, *, #14260, .T. ) ;
#20520 = CIRCLE ( 'NONE', #22028, 5.460999999999938126 ) ;
#20521 = ORIENTED_EDGE ( 'NONE', *, *, #3776, .F. ) ;
#20522 = DIRECTION ( 'NONE',  ( -1.206520773835000154E-12, -1.000000000000000000, 2.336881798973999985E-14 ) ) ;
#20523 = ORIENTED_EDGE ( 'NONE', *, *, #7926, .F. ) ;
#20524 = DIRECTION ( 'NONE',  ( 0.000000000000000000, 0.000000000000000000, -1.000000000000000000 ) ) ;
#20525 = DIRECTION ( 'NONE',  ( 0.000000000000000000, 0.000000000000000000, 1.000000000000000000 ) ) ;
#20526 = ORIENTED_EDGE ( 'NONE', *, *, #22817, .T. ) ;
#20527 = CARTESIAN_POINT ( 'NONE',  ( 145.4150000000009868, -3579.494999999999891, 2246.630000000000109 ) ) ;
#20528 = DIRECTION ( 'NONE',  ( 1.000000000000000000, 0.000000000000000000, 0.000000000000000000 ) ) ;
#20529 = DIRECTION ( 'NONE',  ( 0.000000000000000000, -1.000000000000000000, 0.000000000000000000 ) ) ;
#20530 = APPROVAL_DATE_TIME ( #13163, #15222 ) ;
#20531 = ADVANCED_FACE ( 'NONE', ( #9881 ), #13176, .F. ) ;
#20532 = FACE_OUTER_BOUND ( 'NONE', #2659, .T. ) ;
#20533 = ADVANCED_FACE ( 'NONE', ( #6156 ), #18516, .T. ) ;
#20534 = LINE ( 'NONE', #5723, #1028 ) ;
#20535 = AXIS2_PLACEMENT_3D ( 'NONE', #10016, #3215, #20553 ) ;
#20536 = ADVANCED_FACE ( 'NONE', ( #2519 ), #16802, .T. ) ;
#20537 = EDGE_CURVE ( 'NONE', #19756, #13920, #11529, .T. ) ;
#20538 = LINE ( 'NONE', #18668, #16203 ) ;
#20539 = CARTESIAN_POINT ( 'NONE',  ( 19.05000000000000071, -3656.965000000000146, 2247.392000000000280 ) ) ;
#20540 = ORIENTED_EDGE ( 'NONE', *, *, #20515, .T. ) ;
#20541 = CARTESIAN_POINT ( 'NONE',  ( 137.1118088725371251, -3544.023782198351910, 2255.653223149521637 ) ) ;
#20542 = ORIENTED_EDGE ( 'NONE', *, *, #7949, .T. ) ;
#20543 = CARTESIAN_POINT ( 'NONE',  ( 12.69999999999999929, -3599.497499999999945, 2296.591799999999694 ) ) ;
#20544 = DIRECTION ( 'NONE',  ( 0.000000000000000000, 0.000000000000000000, -1.000000000000000000 ) ) ;
#20545 = EDGE_LOOP ( 'NONE', ( #5963, #20388 ) ) ;
#20546 = ORIENTED_EDGE ( 'NONE', *, *, #10154, .T. ) ;
#20547 = CARTESIAN_POINT ( 'NONE',  ( 55.57575231171000496, -3694.938000000000102, 2275.763800000000174 ) ) ;
#20548 = EDGE_CURVE ( 'NONE', #15612, #20008, #11456, .T. ) ;
#20549 = PLANE ( 'NONE',  #16626 ) ;
#20550 = AXIS2_PLACEMENT_3D ( 'NONE', #12006, #22660, #13775 ) ;
#20551 = DIRECTION ( 'NONE',  ( 0.000000000000000000, 2.336881798971000105E-14, -1.000000000000000000 ) ) ;
#20552 =( REPRESENTATION_RELATIONSHIP ('NONE','NONE', #20448, #13400 ) REPRESENTATION_RELATIONSHIP_WITH_TRANSFORMATION ( #19195 )SHAPE_REPRESENTATION_RELATIONSHIP( ) );
#20553 = DIRECTION ( 'NONE',  ( 0.000000000000000000, 1.000000000000000000, 0.000000000000000000 ) ) ;
#20554 = CARTESIAN_POINT ( 'NONE',  ( 12.69999999999999929, -3590.289999999999964, 2261.593139999999948 ) ) ;
#20555 = CARTESIAN_POINT ( 'NONE',  ( 20.68102893033340095, -3695.646326397317353, 2259.695673346840522 ) ) ;
#20556 = ORIENTED_EDGE ( 'NONE', *, *, #1097, .F. ) ;
#20557 = PERSON_AND_ORGANIZATION ( #5446, #1895 ) ;
#20558 = ORIENTED_EDGE ( 'NONE', *, *, #22759, .F. ) ;
#20559 = CARTESIAN_POINT ( 'NONE',  ( 12.69999999999999929, -3653.789999999999964, 2275.055139999999483 ) ) ;
#20560 = ORIENTED_EDGE ( 'NONE', *, *, #13837, .T. ) ;
#20561 = CIRCLE ( 'NONE', #4474, 0.7619999999999294005 ) ;
#20562 = EDGE_CURVE ( 'NONE', #21589, #5084, #6180, .T. ) ;
#20563 = LINE ( 'NONE', #9785, #13181 ) ;
#20564 = CARTESIAN_POINT ( 'NONE',  ( -6.730999999999872863, -3573.399000000000342, 2247.392000000000280 ) ) ;
#20565 = APPLIED_APPROVAL_ASSIGNMENT ( #2891, ( #3730 ) ) ;
#20566 = VERTEX_POINT ( 'NONE', #1444 ) ;
#20567 = CARTESIAN_POINT ( 'NONE',  ( -6.349999999999999645, -3660.140000000000327, 2247.392000000000280 ) ) ;
#20568 = EDGE_CURVE ( 'NONE', #5428, #17805, #14413, .T. ) ;
#20569 = EDGE_CURVE ( 'NONE', #13134, #9361, #5207, .T. ) ;
#20570 = CARTESIAN_POINT ( 'NONE',  ( 9.524999999998000177, -3694.938000000000102, 2281.351799999999912 ) ) ;
#20571 = CARTESIAN_POINT ( 'NONE',  ( 144.9116092392395672, -3661.850275630491524, 2245.118708807381154 ) ) ;
#20572 = EDGE_LOOP ( 'NONE', ( #16479, #9410, #9632, #16755 ) ) ;
#20573 =( BOUNDED_CURVE ( )  B_SPLINE_CURVE ( 3, ( #2370, #20713, #7762, #4013 ),
 .UNSPECIFIED., .F., .T. ) 
 B_SPLINE_CURVE_WITH_KNOTS ( ( 4, 4 ),
 ( 1.570796327396364100, 3.141592653589738937 ),
 .UNSPECIFIED. ) 
 CURVE ( )  GEOMETRIC_REPRESENTATION_ITEM ( )  RATIONAL_B_SPLINE_CURVE ( ( 1.000000000000000000, 0.8047378542661449696, 0.8047378542661449696, 1.000000000000000000 ) ) 
 REPRESENTATION_ITEM ( '' )  );
#20574 = CARTESIAN_POINT ( 'NONE',  ( 2.859369265564648099, -3695.699999999999818, 2275.763800000091578 ) ) ;
#20575 = CARTESIAN_POINT ( 'NONE',  ( 152.4000000000000057, -3695.699999999999818, 2275.001800000000003 ) ) ;
#20576 = CARTESIAN_POINT ( 'NONE',  ( 127.0000000000000000, -3660.140000000000327, 2250.236800000000130 ) ) ;
#20577 = ORIENTED_EDGE ( 'NONE', *, *, #5868, .T. ) ;
#20578 = EDGE_CURVE ( 'NONE', #11557, #16613, #12166, .T. ) ;
#20579 = CARTESIAN_POINT ( 'NONE',  ( 143.8794601179999972, -3581.600847530791270, 2246.630001408821499 ) ) ;
#20580 = CARTESIAN_POINT ( 'NONE',  ( 15.27310946263999902, -3638.275206607999735, 2279.515940941999816 ) ) ;
#20581 = DIRECTION ( 'NONE',  ( 1.000000000000000000, 0.000000000000000000, 0.000000000000000000 ) ) ;
#20582 = CARTESIAN_POINT ( 'NONE',  ( 15.44495085361937292, -3658.751901201893816, 2249.877081815448491 ) ) ;
#20583 = DIRECTION ( 'NONE',  ( 0.000000000000000000, 0.000000000000000000, -1.000000000000000000 ) ) ;
#20584 = APPROVAL_PERSON_ORGANIZATION ( #4540, #176, #10047 ) ;
#20585 = ORIENTED_EDGE ( 'NONE', *, *, #2150, .F. ) ;
#20586 = APPROVAL_PERSON_ORGANIZATION ( #1190, #17646, #17132 ) ;
#20587 = EDGE_CURVE ( 'NONE', #22767, #13412, #17379, .T. ) ;
#20588 = ORIENTED_EDGE ( 'NONE', *, *, #20942, .F. ) ;
#20589 = AXIS2_PLACEMENT_3D ( 'NONE', #8818, #23093, #14210 ) ;
#20590 = EDGE_CURVE ( 'NONE', #13205, #7536, #8601, .T. ) ;
#20591 = AXIS2_PLACEMENT_3D ( 'NONE', #17128, #6950, #1073 ) ;
#20592 = ORIENTED_EDGE ( 'NONE', *, *, #3070, .T. ) ;
#20593 = CARTESIAN_POINT ( 'NONE',  ( 145.3761992607832383, -3580.159608052688327, 2244.861392947937929 ) ) ;
#20594 = PERSON_AND_ORGANIZATION_ROLE ( 'classification_officer' ) ;
#20595 = CARTESIAN_POINT ( 'NONE',  ( 141.9621417992156864, -3577.760058133676011, 2257.824813613222886 ) ) ;
#20596 = DIRECTION ( 'NONE',  ( -1.000000000000000000, 0.000000000000000000, 0.000000000000000000 ) ) ;
#20597 = DIRECTION ( 'NONE',  ( 0.000000000000000000, -1.000000000000000000, 0.000000000000000000 ) ) ;
#20598 = DIRECTION ( 'NONE',  ( 1.000000000000000000, -2.334777064353000131E-14, -2.343004830739999973E-14 ) ) ;
#20599 = EDGE_CURVE ( 'NONE', #14558, #3088, #22997, .T. ) ;
#20600 = SECURITY_CLASSIFICATION ( '', '', #7199 ) ;
#20601 = CARTESIAN_POINT ( 'NONE',  ( 137.3767596840099259, -3577.852638866662801, 2250.052719895559676 ) ) ;
#20602 = VERTEX_POINT ( 'NONE', #20909 ) ;
#20603 = LOCAL_TIME ( 17, 37, 43.00000000000000000, #13780 ) ;
#20604 = CARTESIAN_POINT ( 'NONE',  ( 15.87499999990501287, -3694.938000000000102, 2281.351800000094954 ) ) ;
#20605 = CARTESIAN_POINT ( 'NONE',  ( 12.69999999999999929, -3582.670000000000073, 2270.760000000000218 ) ) ;
#20606 = EDGE_LOOP ( 'NONE', ( #22417, #20239, #1105, #19462 ) ) ;
#20607 = CARTESIAN_POINT ( 'NONE',  ( 1.270000000000000018, -3695.699999999999818, 2240.279999999999745 ) ) ;
#20608 = CARTESIAN_POINT ( 'NONE',  ( 10.88870223824514838, -3657.311324262453127, 2247.705266899251455 ) ) ;
#20609 = ORIENTED_EDGE ( 'NONE', *, *, #3990, .F. ) ;
#20610 = CIRCLE ( 'NONE', #20258, 2.844800000000001550 ) ;
#20611 = ORIENTED_EDGE ( 'NONE', *, *, #7960, .F. ) ;
#20612 = VERTEX_POINT ( 'NONE', #15638 ) ;
#20613 = DIRECTION ( 'NONE',  ( -1.000000000000000000, 0.000000000000000000, 0.000000000000000000 ) ) ;
#20614 = EDGE_CURVE ( 'NONE', #13646, #8599, #21263, .T. ) ;
#20615 = ORIENTED_EDGE ( 'NONE', *, *, #7834, .F. ) ;
#20616 = DIRECTION ( 'NONE',  ( 0.000000000000000000, 1.000000000000000000, -1.224646799147353207E-16 ) ) ;
#20617 = CARTESIAN_POINT ( 'NONE',  ( -5.588000000000000078, -3694.938000000000102, 2253.487999999999829 ) ) ;
#20618 = DIRECTION ( 'NONE',  ( 0.000000000000000000, 0.000000000000000000, 1.000000000000000000 ) ) ;
#20619 = ORGANIZATION ( 'NAUO-ORG13', 'UNSPECIFIED', 'UNSPECIFIED' ) ;
#20620 = CARTESIAN_POINT ( 'NONE',  ( 141.5231090388281245, -3581.679082975166239, 2247.783365689513630 ) ) ;
#20621 = VERTEX_POINT ( 'NONE', #15754 ) ;
#20622 = DIRECTION ( 'NONE',  ( 0.000000000000000000, 0.000000000000000000, -1.000000000000000000 ) ) ;
#20623 = COORDINATED_UNIVERSAL_TIME_OFFSET ( 0, 0, .AHEAD. ) ;
#20624 = CARTESIAN_POINT ( 'NONE',  ( 130.6067999999989979, -3619.500000000000000, 2239.771999999999935 ) ) ;
#20625 = CARTESIAN_POINT ( 'NONE',  ( 20.71806297877481029, -3543.329302114565053, 2259.603420030892266 ) ) ;
#20626 = CIRCLE ( 'NONE', #13901, 0.7619999999999294005 ) ;
#20627 = FACE_OUTER_BOUND ( 'NONE', #9882, .T. ) ;
#20628 = CIRCLE ( 'NONE', #10535, 0.7619999999999294005 ) ;
#20629 = B_SPLINE_CURVE_WITH_KNOTS ( 'NONE', 3,
 ( #285, #2268, #3903, #14227, #1804, #14464 ),
 .UNSPECIFIED., .F., .F.,
 ( 4, 1, 1, 4 ),
 ( 0.000000000000000000, 0.3333333333333000081, 0.6666666666667000474, 1.000000000000000000 ),
 .UNSPECIFIED. ) ;
#20630 = ORIENTED_EDGE ( 'NONE', *, *, #22517, .F. ) ;
#20631 = APPROVAL ( #10630, 'UNKNOWN' ) ;
#20632 = VERTEX_POINT ( 'NONE', #22879 ) ;
#20633 = VERTEX_POINT ( 'NONE', #17614 ) ;
#20634 = CARTESIAN_POINT ( 'NONE',  ( 79.80679999999999552, -3670.300000000000182, 2239.771999999999935 ) ) ;
#20635 = ORIENTED_EDGE ( 'NONE', *, *, #16655, .T. ) ;
#20636 = LINE ( 'NONE', #17123, #4537 ) ;
#20637 = DIRECTION ( 'NONE',  ( 0.000000000000000000, 1.000000000000000000, 0.000000000000000000 ) ) ;
#20638 = AXIS2_PLACEMENT_3D ( 'NONE', #11184, #6145, #16790 ) ;
#20639 = ORIENTED_EDGE ( 'NONE', *, *, #8387, .T. ) ;
#20640 = TOROIDAL_SURFACE ( 'NONE', #17279, 1.905000000000000027, 1.270000000000000018 ) ;
#20641 = DIRECTION ( 'NONE',  ( 0.000000000000000000, 0.000000000000000000, -1.000000000000000000 ) ) ;
#20642 =( NAMED_UNIT ( * ) SI_UNIT ( $, .STERADIAN. ) SOLID_ANGLE_UNIT ( ) );
#20643 = CARTESIAN_POINT ( 'NONE',  ( -6.349999999999999645, -3578.860000000000127, 2247.392000000000280 ) ) ;
#20644 = CARTESIAN_POINT ( 'NONE',  ( 114.2999999999999972, -3644.899999999999636, 2259.837999999999738 ) ) ;
#20645 = SECURITY_CLASSIFICATION_LEVEL ( 'unclassified' ) ;
#20646 = CARTESIAN_POINT ( 'NONE',  ( 12.69997932225824400, -3596.652698770999905, 2279.817639835496266 ) ) ;
#20647 = CARTESIAN_POINT ( 'NONE',  ( 12.69999999999999929, -3599.497499999999945, 2295.829799999999977 ) ) ;
#20648 = VECTOR ( 'NONE', #22320, 1000.000000000000000 ) ;
#20649 = CARTESIAN_POINT ( 'NONE',  ( 142.3397478532754405, -3658.444484825467953, 2249.676348100301766 ) ) ;
#20650 = DIRECTION ( 'NONE',  ( 0.000000000000000000, -1.000000000000000000, 0.000000000000000000 ) ) ;
#20651 = CIRCLE ( 'NONE', #864, 0.7619999999999279572 ) ;
#20652 = ORIENTED_EDGE ( 'NONE', *, *, #4293, .T. ) ;
#20653 = AXIS2_PLACEMENT_3D ( 'NONE', #10402, #14165, #15681 ) ;
#20654 = CARTESIAN_POINT ( 'NONE',  ( 136.8943284708507804, -3543.452888079240893, 2255.108476224739206 ) ) ;
#20655 = APPROVAL ( #15416, 'UNSPECIFIED' ) ;
#20656 = VECTOR ( 'NONE', #15556, 1000.000000000000000 ) ;
#20657 = ORIENTED_EDGE ( 'NONE', *, *, #10421, .T. ) ;
#20658 = CARTESIAN_POINT ( 'NONE',  ( -12.54218463261993577, -3581.552400000410671, 2247.392000000001190 ) ) ;
#20659 = CARTESIAN_POINT ( 'NONE',  ( 10.36831320285999958, -3660.851200000000063, 2239.391000000000076 ) ) ;
#20660 = ADVANCED_FACE ( 'NONE', ( #8371 ), #3202, .F. ) ;
#20661 = VERTEX_POINT ( 'NONE', #13640 ) ;
#20662 = VERTEX_POINT ( 'NONE', #14114 ) ;
#20663 = DIRECTION ( 'NONE',  ( 1.000000000000000000, 0.000000000000000000, 0.000000000000000000 ) ) ;
#20664 = EDGE_CURVE ( 'NONE', #17982, #12834, #21027, .T. ) ;
#20665 = CARTESIAN_POINT ( 'NONE',  ( 12.70000000000855955, -3582.369629489642193, 2239.010000000067976 ) ) ;
#20666 = CIRCLE ( 'NONE', #1213, 5.714999999999970548 ) ;
#20667 = DIRECTION ( 'NONE',  ( 0.000000000000000000, 0.000000000000000000, 1.000000000000000000 ) ) ;
#20668 = EDGE_CURVE ( 'NONE', #3271, #16691, #3542, .T. ) ;
#20669 = EDGE_LOOP ( 'NONE', ( #9259, #12060 ) ) ;
#20670 = CARTESIAN_POINT ( 'NONE',  ( 139.6999999999999886, -3581.400000000000091, 2272.030000000000200 ) ) ;
#20671 = DIRECTION ( 'NONE',  ( 1.000000000000000000, 0.000000000000000000, 0.000000000000000000 ) ) ;
#20672 = DIRECTION ( 'NONE',  ( 1.224646799147353207E-16, 1.000000000000000000, -0.000000000000000000 ) ) ;
#20673 = AXIS2_PLACEMENT_3D ( 'NONE', #15183, #18921, #20796 ) ;
#20674 = CARTESIAN_POINT ( 'NONE',  ( -12.31899999999987294, -3573.399000000000342, 2247.392000000000280 ) ) ;
#20675 = ORIENTED_EDGE ( 'NONE', *, *, #13290, .T. ) ;
#20676 = SECURITY_CLASSIFICATION_LEVEL ( 'unclassified' ) ;
#20677 = AXIS2_PLACEMENT_3D ( 'NONE', #657, #7808, #14849 ) ;
#20678 = EDGE_LOOP ( 'NONE', ( #8813, #4202 ) ) ;
#20679 = EDGE_CURVE ( 'NONE', #17291, #20138, #6971, .T. ) ;
#20680 = DIRECTION ( 'NONE',  ( -1.000000000000000000, 0.000000000000000000, 0.000000000000000000 ) ) ;
#20681 = DIRECTION ( 'NONE',  ( 1.000000000000000000, 0.000000000000000000, 0.000000000000000000 ) ) ;
#20682 = DIRECTION ( 'NONE',  ( 0.000000000000000000, -1.000000000000000000, 0.000000000000000000 ) ) ;
#20683 = EDGE_CURVE ( 'NONE', #2780, #17291, #8476, .T. ) ;
#20684 = EDGE_LOOP ( 'NONE', ( #6336, #5190, #14937, #7832 ) ) ;
#20685 = VECTOR ( 'NONE', #17923, 1000.000000000000000 ) ;
#20686 = DIRECTION ( 'NONE',  ( 1.000000000000000000, 0.000000000000000000, 3.680805717774999826E-13 ) ) ;
#20687 = DIRECTION ( 'NONE',  ( 0.000000000000000000, -1.000000000000000000, 0.000000000000000000 ) ) ;
#20688 = CARTESIAN_POINT ( 'NONE',  ( 144.7271686052660300, -3662.223246664079397, 2245.454731745688150 ) ) ;
#20689 = B_SPLINE_CURVE_WITH_KNOTS ( 'NONE', 3,
 ( #10406, #8654, #19550, #22929, #6904, #21201, #19435, #8772, #29, #1785, #10687, #6637, #4747, #13531, #19596, #8264, #17158, #12008, #9889 ),
 .UNSPECIFIED., .F., .F.,
 ( 4, 2, 2, 1, 2, 2, 2, 2, 2, 4 ),
 ( 0.000000000000000000, 0.1250000000003315404, 0.1875000000007193135, 0.2187500000009131862, 0.2343750000008835155, 0.2500000000008538725, 0.3750000000007115419, 0.5000000000005692113, 0.7500000000002845502, 1.000000000000000000 ),
 .UNSPECIFIED. ) ;
#20690 = VERTEX_POINT ( 'NONE', #10352 ) ;
#20691 = TOROIDAL_SURFACE ( 'NONE', #9121, 5.080000000000000071, 0.3810000000000000053 ) ;
#20692 = CARTESIAN_POINT ( 'NONE',  ( 139.6999999999999886, -3581.400000000000091, 2270.760000000000218 ) ) ;
#20693 = CARTESIAN_POINT ( 'NONE',  ( 14.06056753155343308, -3662.003450156426425, 2249.541530534452249 ) ) ;
#20694 = CIRCLE ( 'NONE', #3877, 5.460999999999938126 ) ;
#20695 = DIRECTION ( 'NONE',  ( 0.000000000000000000, -1.000000000000000000, 0.000000000000000000 ) ) ;
#20696 = VERTEX_POINT ( 'NONE', #3438 ) ;
#20697 = FACE_OUTER_BOUND ( 'NONE', #6104, .T. ) ;
#20698 = CARTESIAN_POINT ( 'NONE',  ( 12.70000000000085727, -3636.657698770567094, 2279.817639764978139 ) ) ;
#20699 = ADVANCED_FACE ( 'NONE', ( #6854 ), #22618, .T. ) ;
#20700 = CARTESIAN_POINT ( 'NONE',  ( 133.9967742479666697, -3579.071087744469878, 2244.547217120886671 ) ) ;
#20701 = CARTESIAN_POINT ( 'NONE',  ( 15.40608766543241082, -3658.626372987976538, 2249.801193023435189 ) ) ;
#20702 = CARTESIAN_POINT ( 'NONE',  ( 114.2999999999999972, -3594.099999999999909, 2239.771999999999935 ) ) ;
#20703 = VERTEX_POINT ( 'NONE', #11997 ) ;
#20704 = VECTOR ( 'NONE', #7054, 999.9999999999998863 ) ;
#20705 = EDGE_LOOP ( 'NONE', ( #13876, #14229, #14466, #15205 ) ) ;
#20706 = EDGE_CURVE ( 'NONE', #4559, #22295, #9591, .T. ) ;
#20707 = ADVANCED_FACE ( 'NONE', ( #22531 ), #6502, .T. ) ;
#20708 = CARTESIAN_POINT ( 'NONE',  ( 98.75520000000000209, -3568.700000000000273, 2259.837999999999738 ) ) ;
#20709 = ORIENTED_EDGE ( 'NONE', *, *, #15407, .F. ) ;
#20710 = CARTESIAN_POINT ( 'NONE',  ( 15.54479972192533488, -3579.494999998566982, 2257.962943247991461 ) ) ;
#20711 = DATE_AND_TIME ( #6321, #12368 ) ;
#20712 = AXIS2_PLACEMENT_3D ( 'NONE', #1648, #17701, #8806 ) ;
#20713 = CARTESIAN_POINT ( 'NONE',  ( -12.69999999986577244, -3580.297314745182575, 2244.902497835854319 ) ) ;
#20714 = CARTESIAN_POINT ( 'NONE',  ( 142.5447999999989861, -3579.494999999999891, 2257.962944264955695 ) ) ;
#20715 = CARTESIAN_POINT ( 'NONE',  ( 54.40679999999999694, -3568.700000000000273, 2260.600000000000364 ) ) ;
#20716 =( BOUNDED_CURVE ( )  B_SPLINE_CURVE ( 3, ( #8968, #19984, #3917, #7100 ),
 .UNSPECIFIED., .F., .T. ) 
 B_SPLINE_CURVE_WITH_KNOTS ( ( 4, 4 ),
 ( 4.051959034059917173E-16, 1.570796326195641912 ),
 .UNSPECIFIED. ) 
 CURVE ( )  GEOMETRIC_REPRESENTATION_ITEM ( )  RATIONAL_B_SPLINE_CURVE ( ( 1.000000000000000000, 0.8047378542656107303, 0.8047378542656107303, 1.000000000000000000 ) ) 
 REPRESENTATION_ITEM ( '' )  );
#20717 = CARTESIAN_POINT ( 'NONE',  ( 20.32000000000000028, -3694.938000000000102, 2285.606299999999919 ) ) ;
#20718 = CIRCLE ( 'NONE', #9809, 5.079999999999973426 ) ;
#20719 = CARTESIAN_POINT ( 'NONE',  ( 137.8138258362651811, -3577.363333663654430, 2249.812340048487840 ) ) ;
#20720 = EDGE_LOOP ( 'NONE', ( #8467, #8225, #12482, #2666 ) ) ;
#20721 = CIRCLE ( 'NONE', #9506, 3.606799999999001027 ) ;
#20722 = EDGE_CURVE ( 'NONE', #15342, #10158, #15524, .T. ) ;
#20723 = CARTESIAN_POINT ( 'NONE',  ( 12.69999999999999929, -3639.502500000000055, 2264.841800000000148 ) ) ;
#20724 = CARTESIAN_POINT ( 'NONE',  ( 144.7800000000000011, -3659.504999999999654, 2244.978999999999814 ) ) ;
#20725 = VERTEX_POINT ( 'NONE', #2159 ) ;
#20726 = CARTESIAN_POINT ( 'NONE',  ( 151.4000000000000057, -3660.140000000000327, 2247.392000000000280 ) ) ;
#20727 = CARTESIAN_POINT ( 'NONE',  ( 10.81816717404539219, -3657.371485001214296, 2248.046767603714216 ) ) ;
#20728 = EDGE_LOOP ( 'NONE', ( #19846, #17774, #20151, #17342 ) ) ;
#20729 = ORIENTED_EDGE ( 'NONE', *, *, #21685, .F. ) ;
#20730 = LINE ( 'NONE', #11945, #15791 ) ;
#20731 = PRODUCT_DEFINITION_CONTEXT ( 'detailed design', #18170, 'design' ) ;
#20732 = ORIENTED_EDGE ( 'NONE', *, *, #559, .T. ) ;
#20733 = EDGE_CURVE ( 'NONE', #17585, #3143, #20629, .T. ) ;
#20734 = EDGE_CURVE ( 'NONE', #4633, #7148, #10286, .T. ) ;
#20735 = DIRECTION ( 'NONE',  ( -1.000000000000000000, -2.590196616239000129E-13, 3.885294924357999613E-13 ) ) ;
#20736 = EDGE_CURVE ( 'NONE', #9068, #1906, #5431, .T. ) ;
#20737 = DIRECTION ( 'NONE',  ( 0.000000000000000000, 0.000000000000000000, -1.000000000000000000 ) ) ;
#20738 = CARTESIAN_POINT ( 'NONE',  ( 0.000000000000000000, 0.000000000000000000, 0.000000000000000000 ) ) ;
#20739 = EDGE_CURVE ( 'NONE', #4457, #18481, #8421, .T. ) ;
#20740 = CARTESIAN_POINT ( 'NONE',  ( 141.8047404989038682, -3581.408896080104114, 2248.655369336666809 ) ) ;
#20741 = ORIENTED_EDGE ( 'NONE', *, *, #2364, .F. ) ;
#20742 = CARTESIAN_POINT ( 'NONE',  ( 138.4354735775639256, -3582.050017445782032, 2257.663486765196467 ) ) ;
#20743 = CIRCLE ( 'NONE', #20372, 0.3809999999999647002 ) ;
#20744 = APPROVAL_STATUS ( 'not_yet_approved' ) ;
#20745 = AXIS2_PLACEMENT_3D ( 'NONE', #10004, #21346, #23083 ) ;
#20746 = AXIS2_PLACEMENT_3D ( 'NONE', #14727, #19643, #12621 ) ;
#20747 = DIRECTION ( 'NONE',  ( 1.224646799147353207E-16, 1.000000000000000000, -0.000000000000000000 ) ) ;
#20748 = CARTESIAN_POINT ( 'NONE',  ( 20.66921499434370091, -3543.363127659929887, 2259.725433999880352 ) ) ;
#20749 = EDGE_CURVE ( 'NONE', #21667, #3669, #14780, .T. ) ;
#20750 = DIRECTION ( 'NONE',  ( 0.000000000000000000, 0.000000000000000000, -1.000000000000000000 ) ) ;
#20751 = ORIENTED_EDGE ( 'NONE', *, *, #13868, .F. ) ;
#20752 = DIRECTION ( 'NONE',  ( 2.185478394942999951E-13, 1.295098308114000000E-13, 1.000000000000000000 ) ) ;
#20753 = EDGE_CURVE ( 'NONE', #2102, #8915, #7084, .T. ) ;
#20754 = EDGE_CURVE ( 'NONE', #15794, #10464, #15584, .T. ) ;
#20755 = ORIENTED_EDGE ( 'NONE', *, *, #7802, .F. ) ;
#20756 = AXIS2_PLACEMENT_3D ( 'NONE', #22766, #1563, #1324 ) ;
#20757 = CARTESIAN_POINT ( 'NONE',  ( 40.94480000000000075, -3594.099999999999909, 2261.869999999999891 ) ) ;
#20758 = AXIS2_PLACEMENT_3D ( 'NONE', #18394, #22022, #13018 ) ;
#20759 = AXIS2_PLACEMENT_3D ( 'NONE', #19768, #16010, #189 ) ;
#20760 = CARTESIAN_POINT ( 'NONE',  ( 12.70000000000855955, -3662.379629489641502, 2239.010000000067976 ) ) ;
#20761 = AXIS2_PLACEMENT_3D ( 'NONE', #17153, #13071, #14950 ) ;
#20762 = ORIENTED_EDGE ( 'NONE', *, *, #8801, .T. ) ;
#20763 = CARTESIAN_POINT ( 'NONE',  ( -12.69999999999999929, -3661.706170452999686, 2250.104686796999886 ) ) ;
#20764 = CARTESIAN_POINT ( 'NONE',  ( 127.0000000000000000, -3619.500000000000000, 2259.837999999999738 ) ) ;
#20765 = ORIENTED_EDGE ( 'NONE', *, *, #22679, .T. ) ;
#20766 = LINE ( 'NONE', #17243, #21448 ) ;
#20767 = DIRECTION ( 'NONE',  ( 0.000000000000000000, 0.000000000000000000, -1.000000000000000000 ) ) ;
#20768 = CARTESIAN_POINT ( 'NONE',  ( 13.01510455369341557, -3602.330645362285395, 2279.814648973302610 ) ) ;
#20769 = CARTESIAN_POINT ( 'NONE',  ( 15.24000000000000021, -3694.430000000000291, 2255.774000000000342 ) ) ;
#20770 = CALENDAR_DATE ( 2026, 26, 10 ) ;
#20771 = CARTESIAN_POINT ( 'NONE',  ( 6.996957829346665214, -3659.928346034561400, 2244.547218180292020 ) ) ;
#20772 = CARTESIAN_POINT ( 'NONE',  ( 139.6999999999999886, -3659.504999999999654, 2272.030000000000200 ) ) ;
#20773 = CARTESIAN_POINT ( 'NONE',  ( 88.90000000000000568, -3644.899999999999636, 2259.837999999999738 ) ) ;
#20774 = CIRCLE ( 'NONE', #16295, 0.3809999999999647002 ) ;
#20775 = CIRCLE ( 'NONE', #18915, 5.080000000000000071 ) ;
#20776 = CARTESIAN_POINT ( 'NONE',  ( 95.25000000000000000, -3670.300000000000182, 2250.236800000000130 ) ) ;
#20777 = DIRECTION ( 'NONE',  ( -1.000000000000000000, 0.000000000000000000, 0.000000000000000000 ) ) ;
#20778 = AXIS2_PLACEMENT_3D ( 'NONE', #1539, #12210, #4711 ) ;
#20779 = VERTEX_POINT ( 'NONE', #12812 ) ;
#20780 = LINE ( 'NONE', #17144, #8114 ) ;
#20781 = VERTEX_POINT ( 'NONE', #12926 ) ;
#20782 = CARTESIAN_POINT ( 'NONE',  ( 4.878091718509972807, -3695.444958114254405, 2260.094543566995071 ) ) ;
#20783 = DIRECTION ( 'NONE',  ( -0.6887494619132868978, 0.000000000000000000, 0.7249994335957496983 ) ) ;
#20784 = EDGE_LOOP ( 'NONE', ( #16157, #19666, #20915, #22026 ) ) ;
#20785 = ORIENTED_EDGE ( 'NONE', *, *, #4770, .T. ) ;
#20786 = CARTESIAN_POINT ( 'NONE',  ( 54.40679999999999694, -3670.300000000000182, 2239.009999999999764 ) ) ;
#20787 = CIRCLE ( 'NONE', #17417, 0.7620000000000000107 ) ;
#20788 = DIRECTION ( 'NONE',  ( -1.000000000000000000, 1.351868168142999859E-13, 0.000000000000000000 ) ) ;
#20789 = CIRCLE ( 'NONE', #18190, 3.175000000000149925 ) ;
#20790 = DIRECTION ( 'NONE',  ( 1.000000000000000000, 0.000000000000000000, 0.000000000000000000 ) ) ;
#20791 = EDGE_LOOP ( 'NONE', ( #22452, #5205 ) ) ;
#20792 = VECTOR ( 'NONE', #13008, 1000.000000000000000 ) ;
#20793 = DIRECTION ( 'NONE',  ( 1.224646799141920914E-16, -1.000000000000000000, -2.336881798971000421E-14 ) ) ;
#20794 = CARTESIAN_POINT ( 'NONE',  ( 15.03168679714165634, -3638.156299999853218, 2296.433984632644751 ) ) ;
#20795 = AXIS2_PLACEMENT_3D ( 'NONE', #3029, #3374, #17790 ) ;
#20796 = DIRECTION ( 'NONE',  ( 1.000000000000000000, 0.000000000000000000, 0.000000000000000000 ) ) ;
#20797 = CARTESIAN_POINT ( 'NONE',  ( 137.2160575470620927, -3658.069772174391346, 2257.872821556948566 ) ) ;
#20798 = CARTESIAN_POINT ( 'NONE',  ( 20.57350643676103630, -3695.530403268316604, 2259.964929154887614 ) ) ;
#20799 = VERTEX_POINT ( 'NONE', #19967 ) ;
#20800 = COORDINATED_UNIVERSAL_TIME_OFFSET ( 0, 0, .AHEAD. ) ;
#20801 = APPLIED_DATE_AND_TIME_ASSIGNMENT ( #17457, #11842, ( #6739 ) ) ;
#20802 = EDGE_CURVE ( 'NONE', #17234, #2120, #4662, .T. ) ;
#20803 = ORIENTED_EDGE ( 'NONE', *, *, #4852, .T. ) ;
#20804 = VECTOR ( 'NONE', #12102, 1000.000000000000000 ) ;
#20805 = DIRECTION ( 'NONE',  ( -1.000000000000000000, 0.000000000000000000, 0.000000000000000000 ) ) ;
#20806 = CARTESIAN_POINT ( 'NONE',  ( 10.68286790803779773, -3581.501839941320668, 2248.451798419007901 ) ) ;
#20807 = EDGE_CURVE ( 'NONE', #204, #22999, #20086, .T. ) ;
#20808 = LINE ( 'NONE', #15077, #6353 ) ;
#20809 = ADVANCED_FACE ( 'NONE', ( #19848 ), #14348, .F. ) ;
#20810 = CIRCLE ( 'NONE', #608, 1.269999999999993356 ) ;
#20811 = ORIENTED_EDGE ( 'NONE', *, *, #4359, .T. ) ;
#20812 = VECTOR ( 'NONE', #4735, 1000.000000000000000 ) ;
#20813 = FACE_BOUND ( 'NONE', #5237, .T. ) ;
#20814 = ADVANCED_FACE ( 'NONE', ( #18200 ), #9065, .T. ) ;
#20815 = AXIS2_PLACEMENT_3D ( 'NONE', #1216, #22773, #1452 ) ;
#20816 = DIRECTION ( 'NONE',  ( 0.000000000000000000, 1.000000000000000000, 0.000000000000000000 ) ) ;
#20817 = CARTESIAN_POINT ( 'NONE',  ( 144.5620013165544151, -3662.508668946073612, 2245.816465486211655 ) ) ;
#20818 = DIRECTION ( 'NONE',  ( 0.000000000000000000, -1.000000000000000000, 0.000000000000000000 ) ) ;
#20819 = CIRCLE ( 'NONE', #17430, 0.7619999999999294005 ) ;
#20820 = PLANE ( 'NONE',  #545 ) ;
#20821 = LINE ( 'NONE', #6416, #1332 ) ;
#20822 = AXIS2_PLACEMENT_3D ( 'NONE', #18595, #16828, #4417 ) ;
#20823 = VERTEX_POINT ( 'NONE', #15984 ) ;
#20824 = EDGE_CURVE ( 'NONE', #11488, #9357, #16636, .T. ) ;
#20825 = B_SPLINE_CURVE_WITH_KNOTS ( 'NONE', 3,
 ( #10193, #20981, #17333, #8566, #15708, #6810, #3393, #1055, #22489, #8210, #6463, #13602, #20742, #4690, #2936, #10073, #16282, #14415 ),
 .UNSPECIFIED., .F., .F.,
 ( 4, 2, 2, 2, 2, 2, 2, 2, 4 ),
 ( 0.01338853779424258733, 0.01394642552155045574, 0.01450431324885832415, 0.01506220097616619430, 0.01562008870347406271, 0.01617797643078193112, 0.01673586415808980127, 0.01729375188539766794, 0.01785163961270553809 ),
 .UNSPECIFIED. ) ;
#20826 = LINE ( 'NONE', #20476, #3569 ) ;
#20827 = CARTESIAN_POINT ( 'NONE',  ( 15.54479999999999862, -3639.502500000000055, 2279.447335734999797 ) ) ;
#20828 = CARTESIAN_POINT ( 'NONE',  ( 12.69999999999999929, -3589.528000000000247, 2268.705139999999574 ) ) ;
#20829 = CARTESIAN_POINT ( 'NONE',  ( 10.92571717110000051, -3597.265967912000178, 2279.676081828000406 ) ) ;
#20830 = LINE ( 'NONE', #8410, #20656 ) ;
#20831 = ORIENTED_EDGE ( 'NONE', *, *, #11381, .F. ) ;
#20832 = ORIENTED_EDGE ( 'NONE', *, *, #19119, .T. ) ;
#20833 = TOROIDAL_SURFACE ( 'NONE', #2143, 4.114799999999999791, 1.270000000000000018 ) ;
#20834 = ORIENTED_EDGE ( 'NONE', *, *, #6839, .F. ) ;
#20835 = CARTESIAN_POINT ( 'NONE',  ( 142.1683190381772590, -3658.078567413148448, 2257.869726351763802 ) ) ;
#20836 = CALENDAR_DATE ( 2026, 26, 10 ) ;
#20837 = LINE ( 'NONE', #8886, #21793 ) ;
#20838 = ORIENTED_EDGE ( 'NONE', *, *, #16559, .T. ) ;
#20839 = ADVANCED_FACE ( 'NONE', ( #8951 ), #19642, .T. ) ;
#20840 = CARTESIAN_POINT ( 'NONE',  ( 12.69999999999999929, -3579.494999999999891, 2272.030000000000200 ) ) ;
#20841 = CYLINDRICAL_SURFACE ( 'NONE', #5474, 5.714999999998998881 ) ;
#20842 = EDGE_CURVE ( 'NONE', #14926, #16048, #3780, .T. ) ;
#20843 = DIRECTION ( 'NONE',  ( 0.000000000000000000, 0.000000000000000000, 1.000000000000000000 ) ) ;
#20844 = EDGE_CURVE ( 'NONE', #11974, #22650, #20774, .T. ) ;
#20845 = DIRECTION ( 'NONE',  ( 0.000000000000000000, 0.000000000000000000, 1.000000000000000000 ) ) ;
#20846 = DIRECTION ( 'NONE',  ( -0.5000000000048030468, 0.8660254037816655925, 0.000000000000000000 ) ) ;
#20847 = EDGE_LOOP ( 'NONE', ( #22497, #21810, #7771, #5394 ) ) ;
#20848 = CIRCLE ( 'NONE', #5895, 3.606799999999001027 ) ;
#20849 = DIRECTION ( 'NONE',  ( 0.000000000000000000, -1.000000000000000000, 0.000000000000000000 ) ) ;
#20850 = CIRCLE ( 'NONE', #15619, 0.7619999999999294005 ) ;
#20851 = LINE ( 'NONE', #16859, #17782 ) ;
#20852 = ORIENTED_EDGE ( 'NONE', *, *, #16840, .T. ) ;
#20853 = CARTESIAN_POINT ( 'NONE',  ( 147.8270794805000037, -3695.699999999999818, 2259.329999999999927 ) ) ;
#20854 = CARTESIAN_POINT ( 'NONE',  ( -0.7620000000000000107, -3544.061999999999898, 2253.487999999999829 ) ) ;
#20855 = ORIENTED_EDGE ( 'NONE', *, *, #12993, .F. ) ;
#20856 = AXIS2_PLACEMENT_3D ( 'NONE', #4809, #6584, #6812 ) ;
#20857 = ORIENTED_EDGE ( 'NONE', *, *, #22964, .F. ) ;
#20858 = DIRECTION ( 'NONE',  ( 1.000000000000000000, 0.000000000000000000, 0.000000000000000000 ) ) ;
#20859 = EDGE_CURVE ( 'NONE', #13662, #13759, #22637, .T. ) ;
#20860 = ORIENTED_EDGE ( 'NONE', *, *, #4376, .T. ) ;
#20861 = DIRECTION ( 'NONE',  ( 0.000000000000000000, 0.000000000000000000, 1.000000000000000000 ) ) ;
#20862 = CARTESIAN_POINT ( 'NONE',  ( 10.50330237546534207, -3577.685423964297115, 2249.983956755341751 ) ) ;
#20863 = CARTESIAN_POINT ( 'NONE',  ( 0.000000000000000000, 0.000000000000000000, 0.000000000000000000 ) ) ;
#20864 = CARTESIAN_POINT ( 'NONE',  ( 55.57575231171000496, -3544.061999999999898, 2275.763800000000174 ) ) ;
#20865 = VERTEX_POINT ( 'NONE', #8118 ) ;
#20866 = CARTESIAN_POINT ( 'NONE',  ( 131.8858715492527267, -3695.429311327186497, 2260.113811941836957 ) ) ;
#20867 = COORDINATED_UNIVERSAL_TIME_OFFSET ( 0, 0, .AHEAD. ) ;
#20868 = AXIS2_PLACEMENT_3D ( 'NONE', #148, #10688, #19829 ) ;
#20869 = CYLINDRICAL_SURFACE ( 'NONE', #22721, 1.269999999999900098 ) ;
#20870 = EDGE_CURVE ( 'NONE', #21361, #13997, #21899, .T. ) ;
#20871 = CARTESIAN_POINT ( 'NONE',  ( 25.39999999999999858, -3619.500000000000000, 2239.009999999999764 ) ) ;
#20872 = CIRCLE ( 'NONE', #8113, 0.7619999999999987894 ) ;
#20873 = DIRECTION ( 'NONE',  ( 1.000000000000000000, 0.000000000000000000, 0.000000000000000000 ) ) ;
#20874 = ORIENTED_EDGE ( 'NONE', *, *, #19174, .T. ) ;
#20875 = DIRECTION ( 'NONE',  ( 0.000000000000000000, 0.000000000000000000, 1.000000000000000000 ) ) ;
#20876 = ADVANCED_FACE ( 'NONE', ( #7646 ), #18532, .T. ) ;
#20877 =( REPRESENTATION_RELATIONSHIP ('NONE','NONE', #20448, #19840 ) REPRESENTATION_RELATIONSHIP_WITH_TRANSFORMATION ( #1567 )SHAPE_REPRESENTATION_RELATIONSHIP( ) );
#20878 = EDGE_CURVE ( 'NONE', #2067, #17394, #17429, .T. ) ;
#20879 = LINE ( 'NONE', #22184, #22249 ) ;
#20880 = CIRCLE ( 'NONE', #18283, 0.7619999999999987894 ) ;
#20881 = VERTEX_POINT ( 'NONE', #9743 ) ;
#20882 = CARTESIAN_POINT ( 'NONE',  ( 9.524999999997000089, -3544.061999999999898, 2281.351799999999912 ) ) ;
#20883 = AXIS2_PLACEMENT_3D ( 'NONE', #19540, #1963, #10981 ) ;
#20884 = LINE ( 'NONE', #12087, #925 ) ;
#20885 = ORIENTED_EDGE ( 'NONE', *, *, #8058, .F. ) ;
#20886 = ORIENTED_EDGE ( 'NONE', *, *, #17710, .F. ) ;
#20887 = PLANE ( 'NONE',  #12413 ) ;
#20888 = DIRECTION ( 'NONE',  ( 1.000000000000000000, 0.000000000000000000, 0.000000000000000000 ) ) ;
#20889 = EDGE_CURVE ( 'NONE', #11227, #22687, #17397, .T. ) ;
#20890 = ORIENTED_EDGE ( 'NONE', *, *, #22964, .T. ) ;
#20891 = DIRECTION ( 'NONE',  ( 0.000000000000000000, 1.000000000000000000, 0.000000000000000000 ) ) ;
#20892 = CARTESIAN_POINT ( 'NONE',  ( 137.7873330486999919, -3657.399152860999493, 2246.630000000000109 ) ) ;
#20893 = SHAPE_REPRESENTATION_RELATIONSHIP ( 'NONE' , 'NONE' ,  #9499, #6029 ) ;
#20894 = CARTESIAN_POINT ( 'NONE',  ( 15.39424449907000003, -3600.429004351000003, 2279.486256451000372 ) ) ;
#20895 = CARTESIAN_POINT ( 'NONE',  ( 34.49320000000000164, -3644.899999999999636, 2239.771999999999935 ) ) ;
#20896 = EDGE_CURVE ( 'NONE', #18910, #20500, #9902, .T. ) ;
#20897 = PERSON_AND_ORGANIZATION_ROLE ( 'creator' ) ;
#20898 = ADVANCED_FACE ( 'NONE', ( #9860 ), #20194, .F. ) ;
#20899 = CARTESIAN_POINT ( 'NONE',  ( 12.70000000003999929, -3662.197400000000016, 2242.820000000000164 ) ) ;
#20900 = CARTESIAN_POINT ( 'NONE',  ( 12.69999999999999929, -3662.679999999999836, 2270.760000000000218 ) ) ;
#20901 = DIRECTION ( 'NONE',  ( 0.000000000000000000, 0.000000000000000000, -1.000000000000000000 ) ) ;
#20902 = CARTESIAN_POINT ( 'NONE',  ( 141.8231898388004595, -3657.611600801285931, 2248.695890107555897 ) ) ;
#20903 = ORIENTED_EDGE ( 'NONE', *, *, #11548, .F. ) ;
#20904 = CARTESIAN_POINT ( 'NONE',  ( 136.8581536596348087, -3543.408637599010035, 2255.017959195303774 ) ) ;
#20905 = EDGE_CURVE ( 'NONE', #16978, #10242, #6019, .T. ) ;
#20906 = ORIENTED_EDGE ( 'NONE', *, *, #17687, .F. ) ;
#20907 = ORIENTED_EDGE ( 'NONE', *, *, #11519, .F. ) ;
#20908 = DIRECTION ( 'NONE',  ( 0.000000000000000000, 0.000000000000000000, 1.000000000000000000 ) ) ;
#20909 = CARTESIAN_POINT ( 'NONE',  ( 12.69999999999999929, -3604.958499999999731, 2296.210799999999836 ) ) ;
#20910 = ORIENTED_EDGE ( 'NONE', *, *, #21311, .F. ) ;
#20911 = EDGE_LOOP ( 'NONE', ( #20521, #1250, #18062, #3732 ) ) ;
#20912 = DIRECTION ( 'NONE',  ( -0.000000000000000000, 1.000000000000000000, -0.000000000000000000 ) ) ;
#20913 = DIRECTION ( 'NONE',  ( 0.000000000000000000, 0.000000000000000000, -1.000000000000000000 ) ) ;
#20914 = LINE ( 'NONE', #4851, #3595 ) ;
#20915 = ORIENTED_EDGE ( 'NONE', *, *, #8439, .T. ) ;
#20916 = FACE_OUTER_BOUND ( 'NONE', #13687, .T. ) ;
#20917 = CARTESIAN_POINT ( 'NONE',  ( -0.7620000000000000107, -3695.699999999999818, 2253.487999999999829 ) ) ;
#20918 = DIRECTION ( 'NONE',  ( 1.000000000000000000, 1.206643234470999950E-12, 0.000000000000000000 ) ) ;
#20919 = CARTESIAN_POINT ( 'NONE',  ( 95.25000000000000000, -3670.300000000000182, 2247.392000000000280 ) ) ;
#20920 = AXIS2_PLACEMENT_3D ( 'NONE', #9695, #11337, #681 ) ;
#20921 = CARTESIAN_POINT ( 'NONE',  ( 92.50679999999999836, -3594.099999999999909, 2239.009999999999764 ) ) ;
#20922 = EDGE_LOOP ( 'NONE', ( #8411, #19467, #12586, #5274 ) ) ;
#20923 = DATE_TIME_ROLE ( 'creation_date' ) ;
#20924 = EDGE_LOOP ( 'NONE', ( #8250, #14635, #342, #22800 ) ) ;
#20925 = CARTESIAN_POINT ( 'NONE',  ( 35.56000000000000227, -3694.430000000000291, 2247.392000000000280 ) ) ;
#20926 = CARTESIAN_POINT ( 'NONE',  ( 10.89166860073782672, -3581.691115089716277, 2247.681511753725317 ) ) ;
#20927 = VERTEX_POINT ( 'NONE', #4134 ) ;
#20928 = LINE ( 'NONE', #2642, #12704 ) ;
#20929 = ORIENTED_EDGE ( 'NONE', *, *, #1960, .T. ) ;
#20930 = DIRECTION ( 'NONE',  ( 1.224646799147353207E-16, 1.000000000000000000, -0.000000000000000000 ) ) ;
#20931 = AXIS2_PLACEMENT_3D ( 'NONE', #16117, #15658, #67 ) ;
#20932 = DIRECTION ( 'NONE',  ( 0.000000000000000000, 0.000000000000000000, -1.000000000000000000 ) ) ;
#20933 = CARTESIAN_POINT ( 'NONE',  ( 145.2053555853632361, -3661.038792355501755, 2244.692860678725083 ) ) ;
#20934 = AXIS2_PLACEMENT_3D ( 'NONE', #9223, #5600, #18118 ) ;
#20935 = CARTESIAN_POINT ( 'NONE',  ( 12.69999999999999929, -3659.504999999999654, 2239.009999999999764 ) ) ;
#20936 = CARTESIAN_POINT ( 'NONE',  ( 11.49452485132638380, -3662.081945281043318, 2249.471023377334859 ) ) ;
#20937 = APPROVAL ( #10473, 'UNKNOWN' ) ;
#20938 = CARTESIAN_POINT ( 'NONE',  ( 147.4512313346230314, -3543.717426572050044, 2260.271352724699227 ) ) ;
#20939 = VERTEX_POINT ( 'NONE', #18762 ) ;
#20940 = DIRECTION ( 'NONE',  ( -1.000000000000000000, 0.000000000000000000, 0.000000000000000000 ) ) ;
#20941 = DIRECTION ( 'NONE',  ( -1.000000000000000000, 0.000000000000000000, 0.000000000000000000 ) ) ;
#20942 = EDGE_CURVE ( 'NONE', #13900, #1694, #18652, .T. ) ;
#20943 = DIRECTION ( 'NONE',  ( -1.103190638852999933E-12, 1.000000000000000000, 0.000000000000000000 ) ) ;
#20944 = CARTESIAN_POINT ( 'NONE',  ( 15.10427522816852530, -3657.984367098621988, 2249.248490382821274 ) ) ;
#20945 = CARTESIAN_POINT ( 'NONE',  ( 64.76999999999999602, -3544.061999999999898, 2292.819899999999961 ) ) ;
#20946 = ORIENTED_EDGE ( 'NONE', *, *, #13211, .T. ) ;
#20947 = VECTOR ( 'NONE', #6926, 1000.000000000000000 ) ;
#20948 = CARTESIAN_POINT ( 'NONE',  ( 12.69999999999999929, -3590.289999999999964, 2268.705139999999574 ) ) ;
#20949 = LOCAL_TIME ( 17, 37, 43.00000000000000000, #9048 ) ;
#20950 = EDGE_LOOP ( 'NONE', ( #4422, #20886, #12645, #3667 ) ) ;
#20951 = AXIS2_PLACEMENT_3D ( 'NONE', #9193, #16340, #294 ) ;
#20952 = CARTESIAN_POINT ( 'NONE',  ( 139.8886776210838434, -3656.660200000000714, 2257.592639999999392 ) ) ;
#20953 = CALENDAR_DATE ( 2026, 26, 10 ) ;
#20954 = CARTESIAN_POINT ( 'NONE',  ( -8.890000000008001280, -3580.206200000000081, 2249.723686796999573 ) ) ;
#20955 = CARTESIAN_POINT ( 'NONE',  ( 17.77999999999999758, -3599.497499999999945, 2290.241799999999785 ) ) ;
#20956 = DIRECTION ( 'NONE',  ( 0.000000000000000000, -1.000000000000000000, 0.000000000000000000 ) ) ;
#20957 = DIRECTION ( 'NONE',  ( 1.000000000000000000, 0.000000000000000000, 0.000000000000000000 ) ) ;
#20958 = DIRECTION ( 'NONE',  ( -2.324635735433000053E-14, 0.000000000000000000, -1.000000000000000000 ) ) ;
#20959 = CARTESIAN_POINT ( 'NONE',  ( 127.0000000000000000, -3670.300000000000182, 2239.771999999999935 ) ) ;
#20960 = ORIENTED_EDGE ( 'NONE', *, *, #9833, .F. ) ;
#20961 = CARTESIAN_POINT ( 'NONE',  ( -8.890000000006001102, -3661.486200000000281, 2249.723686796999573 ) ) ;
#20962 = PRODUCT_DEFINITION ( 'UNKNOWN', '', #12017, #5972 ) ;
#20963 = LINE ( 'NONE', #3493, #2452 ) ;
#20964 = VERTEX_POINT ( 'NONE', #951 ) ;
#20965 = APPLIED_APPROVAL_ASSIGNMENT ( #4322, ( #11243 ) ) ;
#20966 = DIRECTION ( 'NONE',  ( -1.000000000000000000, 0.000000000000000000, 0.000000000000000000 ) ) ;
#20967 = CARTESIAN_POINT ( 'NONE',  ( 147.3199999999999932, -3694.430000000000291, 2260.600000000000364 ) ) ;
#20968 = ORIENTED_EDGE ( 'NONE', *, *, #5088, .F. ) ;
#20969 = EDGE_CURVE ( 'NONE', #22051, #18481, #21942, .T. ) ;
#20970 = ORIENTED_EDGE ( 'NONE', *, *, #11381, .T. ) ;
#20971 = AXIS2_PLACEMENT_3D ( 'NONE', #3651, #12446, #18179 ) ;
#20972 = CARTESIAN_POINT ( 'NONE',  ( 114.2999999999999972, -3594.099999999999909, 2239.009999999999764 ) ) ;
#20973 = EDGE_CURVE ( 'NONE', #7880, #9083, #19293, .T. ) ;
#20974 = ORIENTED_EDGE ( 'NONE', *, *, #3677, .T. ) ;
#20975 = PRODUCT ( 'Roller 1', 'Roller 1', '', ( #22260 ) ) ;
#20976 = ADVANCED_FACE ( 'NONE', ( #6252 ), #13261, .T. ) ;
#20977 = LINE ( 'NONE', #8561, #8519 ) ;
#20978 = CALENDAR_DATE ( 2026, 26, 10 ) ;
#20979 = CARTESIAN_POINT ( 'NONE',  ( 1.270000000000000018, -3694.430000000000291, 2239.009999999999764 ) ) ;
#20980 = VERTEX_POINT ( 'NONE', #6362 ) ;
#20981 = CARTESIAN_POINT ( 'NONE',  ( 136.8552000000009627, -3579.683686123789812, 2257.962944264955240 ) ) ;
#20982 = APPROVAL_DATE_TIME ( #15476, #16363 ) ;
#20983 = AXIS2_PLACEMENT_3D ( 'NONE', #16600, #5844, #2426 ) ;
#20984 = CARTESIAN_POINT ( 'NONE',  ( 53.64479999999999649, -3670.300000000000182, 2239.771999999999935 ) ) ;
#20985 = APPROVAL_PERSON_ORGANIZATION ( #13221, #7348, #349 ) ;
#20986 = CARTESIAN_POINT ( 'NONE',  ( 14.64183135348199194, -3581.574010930764416, 2248.245069266252358 ) ) ;
#20987 = LOCAL_TIME ( 17, 37, 43.00000000000000000, #3945 ) ;
#20988 = CARTESIAN_POINT ( 'NONE',  ( 134.1794544657873018, -3658.026865190803619, 2245.487007817819176 ) ) ;
#20989 = ADVANCED_FACE ( 'NONE', ( #11609 ), #7323, .T. ) ;
#20990 = DIRECTION ( 'NONE',  ( 1.000000000000000000, 0.000000000000000000, 0.000000000000000000 ) ) ;
#20991 = ORIENTED_EDGE ( 'NONE', *, *, #16650, .F. ) ;
#20992 = CYLINDRICAL_SURFACE ( 'NONE', #14442, 2.844800000000091700 ) ;
#20993 = AXIS2_PLACEMENT_3D ( 'NONE', #9333, #18457, #5478 ) ;
#20994 = DIRECTION ( 'NONE',  ( -1.000000000000000000, -4.815138086611999802E-14, 0.000000000000000000 ) ) ;
#20995 = VERTEX_POINT ( 'NONE', #17004 ) ;
#20996 = DIRECTION ( 'NONE',  ( -1.000000000000000000, 0.000000000000000000, 0.000000000000000000 ) ) ;
#20997 = DIRECTION ( 'NONE',  ( 0.000000000000000000, 0.000000000000000000, 1.000000000000000000 ) ) ;
#20998 = EDGE_LOOP ( 'NONE', ( #6135, #11343, #9550, #12486, #11999 ) ) ;
#20999 = LOCAL_TIME ( 17, 37, 43.00000000000000000, #7360 ) ;
#21000 = DIRECTION ( 'NONE',  ( 0.000000000000000000, 0.000000000000000000, -1.000000000000000000 ) ) ;
#21001 = DIRECTION ( 'NONE',  ( 1.000000000000000000, 0.000000000000000000, 0.000000000000000000 ) ) ;
#21002 = APPLIED_APPROVAL_ASSIGNMENT ( #23090, ( #22059 ) ) ;
#21003 = ORIENTED_EDGE ( 'NONE', *, *, #20878, .F. ) ;
#21004 = EDGE_CURVE ( 'NONE', #22946, #9518, #11417, .T. ) ;
#21005 = FACE_OUTER_BOUND ( 'NONE', #17668, .T. ) ;
#21006 = LINE ( 'NONE', #15621, #1134 ) ;
#21007 = SHAPE_REPRESENTATION_RELATIONSHIP ( 'NONE' , 'NONE' ,  #6985, #15234 ) ;
#21008 = CYLINDRICAL_SURFACE ( 'NONE', #2725, 2.844800000000091700 ) ;
#21010 = DIRECTION ( 'NONE',  ( 0.000000000000000000, 0.000000000000000000, 1.000000000000000000 ) ) ;
#21009 = AXIS2_PLACEMENT_3D ( 'NONE', #21733, #21282, #19863 ) ;
#21011 = DATE_AND_TIME ( #3072, #14963 ) ;
#21012 = EDGE_CURVE ( 'NONE', #10683, #6818, #22264, .T. ) ;
#21013 = VECTOR ( 'NONE', #8120, 1000.000000000000000 ) ;
#21014 = EDGE_CURVE ( 'NONE', #10931, #21665, #15540, .T. ) ;
#21015 = DIRECTION ( 'NONE',  ( 0.000000000000000000, 0.000000000000000000, 1.000000000000000000 ) ) ;
#21016 = CARTESIAN_POINT ( 'NONE',  ( 12.69999999999999929, -3584.956000000000131, 2239.391000000000076 ) ) ;
#21017 = DIRECTION ( 'NONE',  ( 1.000000000000000000, 0.000000000000000000, -1.224646799147353207E-16 ) ) ;
#21018 = CARTESIAN_POINT ( 'NONE',  ( 142.0776493914862897, -3657.942898745972343, 2249.199396469671228 ) ) ;
#21019 = ADVANCED_FACE ( 'NONE', ( #723 ), #8044, .T. ) ;
#21020 = ORIENTED_EDGE ( 'NONE', *, *, #13235, .T. ) ;
#21021 = SPHERICAL_SURFACE ( 'NONE', #17465, 0.7620000000000000107 ) ;
#21022 = ORIENTED_EDGE ( 'NONE', *, *, #21947, .T. ) ;
#21023 = VERTEX_POINT ( 'NONE', #17233 ) ;
#21024 = AXIS2_PLACEMENT_3D ( 'NONE', #7658, #18775, #8132 ) ;
#21025 = EDGE_CURVE ( 'NONE', #16346, #279, #21157, .T. ) ;
#21026 = VECTOR ( 'NONE', #5298, 1000.000000000000000 ) ;
#21027 = LINE ( 'NONE', #13996, #9535 ) ;
#21028 = VERTEX_POINT ( 'NONE', #22744 ) ;
#21029 = ORIENTED_EDGE ( 'NONE', *, *, #15539, .F. ) ;
#21030 = CARTESIAN_POINT ( 'NONE',  ( 4.658066890921409353, -3543.315017898367387, 2259.542481502586270 ) ) ;
#21031 = CARTESIAN_POINT ( 'NONE',  ( 151.1299999999999955, -3695.699999999999818, 2240.279999999999745 ) ) ;
#21032 = DIRECTION ( 'NONE',  ( 1.224646799147353207E-16, 1.000000000000000000, -0.000000000000000000 ) ) ;
#21033 = ORIENTED_EDGE ( 'NONE', *, *, #18244, .T. ) ;
#21034 = DIRECTION ( 'NONE',  ( 0.000000000000000000, -1.000000000000000000, 0.000000000000000000 ) ) ;
#21035 = DIRECTION ( 'NONE',  ( 0.000000000000000000, 0.000000000000000000, -1.000000000000000000 ) ) ;
#21036 = CARTESIAN_POINT ( 'NONE',  ( 138.2734168879149195, -3657.036766217124296, 2257.683488278010373 ) ) ;
#21037 = CARTESIAN_POINT ( 'NONE',  ( 10.78723565514999905, -3581.600816721000228, 2246.630000000000109 ) ) ;
#21038 = AXIS2_PLACEMENT_3D ( 'NONE', #181, #16347, #14248 ) ;
#21039 = VERTEX_POINT ( 'NONE', #3059 ) ;
#21040 = COORDINATED_UNIVERSAL_TIME_OFFSET ( 0, 0, .AHEAD. ) ;
#21041 = ADVANCED_FACE ( 'NONE', ( #1300 ), #22503, .T. ) ;
#21042 = ORIENTED_EDGE ( 'NONE', *, *, #9247, .T. ) ;
#21043 = DIRECTION ( 'NONE',  ( 0.000000000000000000, 0.000000000000000000, -1.000000000000000000 ) ) ;
#21044 = VECTOR ( 'NONE', #14985, 1000.000000000000000 ) ;
#21045 = AXIS2_PLACEMENT_3D ( 'NONE', #10631, #13690, #22580 ) ;
#21046 = CARTESIAN_POINT ( 'NONE',  ( 0.000000000000000000, -3544.570000000000164, 2259.329999999999927 ) ) ;
#21047 = ORIENTED_EDGE ( 'NONE', *, *, #5936, .T. ) ;
#21048 = DIRECTION ( 'NONE',  ( -1.000000000000000000, 0.000000000000000000, 0.000000000000000000 ) ) ;
#21049 = ORIENTED_EDGE ( 'NONE', *, *, #8678, .F. ) ;
#21050 = FACE_BOUND ( 'NONE', #3352, .T. ) ;
#21051 = CARTESIAN_POINT ( 'NONE',  ( -6.349999999999999645, -3544.061999999999898, 2229.612000000000080 ) ) ;
#21052 = CARTESIAN_POINT ( 'NONE',  ( 144.3113860274000047, -3662.880847139000252, 2246.630000000000109 ) ) ;
#21053 = EDGE_CURVE ( 'NONE', #18533, #13134, #14301, .T. ) ;
#21054 = FACE_OUTER_BOUND ( 'NONE', #7375, .T. ) ;
#21055 = CIRCLE ( 'NONE', #7566, 3.606800000000021100 ) ;
#21056 = EDGE_CURVE ( 'NONE', #1809, #22190, #17345, .T. ) ;
#21057 = CARTESIAN_POINT ( 'NONE',  ( 12.01160536040741711, -3662.265695842842433, 2249.282711244598886 ) ) ;
#21058 = LINE ( 'NONE', #19180, #16318 ) ;
#21059 = ORIENTED_EDGE ( 'NONE', *, *, #1235, .T. ) ;
#21060 = DIRECTION ( 'NONE',  ( 0.000000000000000000, 1.000000000000000000, 0.000000000000000000 ) ) ;
#21061 = VECTOR ( 'NONE', #17378, 1000.000000000000000 ) ;
#21062 = DIRECTION ( 'NONE',  ( -1.224646799147353207E-16, 1.000000000000000000, 0.000000000000000000 ) ) ;
#21063 = AXIS2_PLACEMENT_3D ( 'NONE', #12996, #13210, #893 ) ;
#21064 = CARTESIAN_POINT ( 'NONE',  ( 0.7620000000000000107, -3695.699999999999818, 2275.763800000000174 ) ) ;
#21065 = DIRECTION ( 'NONE',  ( 0.000000000000000000, 0.000000000000000000, -1.000000000000000000 ) ) ;
#21066 = DIRECTION ( 'NONE',  ( -2.807875838775999975E-12, 1.000000000000000000, 0.000000000000000000 ) ) ;
#21067 = VERTEX_POINT ( 'NONE', #2948 ) ;
#21068 = CARTESIAN_POINT ( 'NONE',  ( 15.54479999999999862, -3659.504999999999654, 2272.030000000000200 ) ) ;
#21069 = VERTEX_POINT ( 'NONE', #13849 ) ;
#21070 = CARTESIAN_POINT ( 'NONE',  ( 9.842728535705985493, -3543.392327578453205, 2254.979487868655269 ) ) ;
#21072 = VECTOR ( 'NONE', #20077, 1000.000000000000000 ) ;
#21071 = APPROVAL_ROLE ( '' ) ;
#21073 = FACE_OUTER_BOUND ( 'NONE', #13609, .T. ) ;
#21074 = CARTESIAN_POINT ( 'NONE',  ( 101.5999999999999943, -3619.500000000000000, 2260.600000000000364 ) ) ;
#21075 = DIRECTION ( 'NONE',  ( -2.580078660703000173E-14, 3.885294924352999876E-13, -1.000000000000000000 ) ) ;
#21076 = CIRCLE ( 'NONE', #16942, 0.7619999999999294005 ) ;
#21077 = CARTESIAN_POINT ( 'NONE',  ( 12.97550722921000066, -3656.669101291999596, 2257.594923726999696 ) ) ;
#21078 = CARTESIAN_POINT ( 'NONE',  ( 141.0563433985999779, -3657.155744320999929, 2239.391000000000076 ) ) ;
#21079 = AXIS2_PLACEMENT_3D ( 'NONE', #15068, #7687, #2415 ) ;
#21080 = DIRECTION ( 'NONE',  ( 1.000000000000000000, 0.000000000000000000, 0.000000000000000000 ) ) ;
#21081 = ORIENTED_EDGE ( 'NONE', *, *, #2150, .T. ) ;
#21082 = DIRECTION ( 'NONE',  ( -1.000000000000000000, 0.000000000000000000, 0.000000000000000000 ) ) ;
#21083 = MANIFOLD_SOLID_BREP ( 'SOLID259[1]', #3116 ) ;
#21084 = CARTESIAN_POINT ( 'NONE',  ( 9.855199999999999960, -3639.502500000000055, 2281.351799999999912 ) ) ;
#21085 = ORIENTED_EDGE ( 'NONE', *, *, #22900, .T. ) ;
#21086 = CARTESIAN_POINT ( 'NONE',  ( 64.76999999999999602, -3544.061999999999898, 2286.368300000000090 ) ) ;
#21087 = PERSON ( 'NAUO-PER5', 'UNSPECIFIED', 'UNSPECIFIED', ('UNSPECIFIED'), ('UNSPECIFIED'), ('UNSPECIFIED') ) ;
#21088 = CARTESIAN_POINT ( 'NONE',  ( 9.855099624826999971, -3659.505002774999411, 2250.165042250000170 ) ) ;
#21089 = AXIS2_PLACEMENT_3D ( 'NONE', #4097, #4328, #18389 ) ;
#21090 = VERTEX_POINT ( 'NONE', #21116 ) ;
#21091 = CARTESIAN_POINT ( 'NONE',  ( 134.2981814352962999, -3581.361247027981335, 2246.035952059839019 ) ) ;
#21092 = VECTOR ( 'NONE', #17565, 1000.000000000000000 ) ;
#21093 = ORIENTED_EDGE ( 'NONE', *, *, #3770, .T. ) ;
#21094 = CIRCLE ( 'NONE', #15469, 6.349999999999855760 ) ;
#21095 = FACE_OUTER_BOUND ( 'NONE', #5012, .T. ) ;
#21096 = APPROVAL_ROLE ( '' ) ;
#21097 = CARTESIAN_POINT ( 'NONE',  ( 1.270000000000000018, -3695.699999999999818, 2240.279999999999745 ) ) ;
#21098 = VERTEX_POINT ( 'NONE', #5060 ) ;
#21099 = CARTESIAN_POINT ( 'NONE',  ( 131.5729205195000020, -3695.699999999999818, 2259.329999999999927 ) ) ;
#21100 = SECURITY_CLASSIFICATION_LEVEL ( 'unclassified' ) ;
#21101 = PRODUCT_RELATED_PRODUCT_CATEGORY ( 'detail', '', ( #6959 ) ) ;
#21102 = CARTESIAN_POINT ( 'NONE',  ( 12.69999999971559212, -3596.365159094870251, 2296.591799999999694 ) ) ;
#21103 = DIRECTION ( 'NONE',  ( 0.000000000000000000, 0.000000000000000000, -1.000000000000000000 ) ) ;
#21104 = VECTOR ( 'NONE', #14332, 1000.000000000000000 ) ;
#21105 = CARTESIAN_POINT ( 'NONE',  ( 134.1374959654496308, -3658.193646307140625, 2245.317243222136312 ) ) ;
#21106 = EDGE_CURVE ( 'NONE', #22211, #19405, #21237, .T. ) ;
#21107 = EDGE_CURVE ( 'NONE', #12370, #19652, #4680, .T. ) ;
#21108 = DIRECTION ( 'NONE',  ( 0.000000000000000000, 0.000000000000000000, -1.000000000000000000 ) ) ;
#21109 = ORIENTED_EDGE ( 'NONE', *, *, #11994, .T. ) ;
#21110 = DIRECTION ( 'NONE',  ( 0.000000000000000000, 0.000000000000000000, -1.000000000000000000 ) ) ;
#21111 = ADVANCED_FACE ( 'NONE', ( #8346 ), #6571, .T. ) ;
#21112 = ORIENTED_EDGE ( 'NONE', *, *, #19476, .T. ) ;
#21113 = LINE ( 'NONE', #12548, #3172 ) ;
#21114 = VERTEX_POINT ( 'NONE', #6942 ) ;
#21115 = CARTESIAN_POINT ( 'NONE',  ( 38.10000000000000142, -3594.099999999999909, 2261.869999999999891 ) ) ;
#21116 = CARTESIAN_POINT ( 'NONE',  ( 105.2067999999999870, -3670.300000000000182, 2239.009999999999764 ) ) ;
#21117 = ORIENTED_EDGE ( 'NONE', *, *, #9825, .T. ) ;
#21118 = ADVANCED_FACE ( 'NONE', ( #3175 ), #15487, .T. ) ;
#21119 = FACE_OUTER_BOUND ( 'NONE', #9113, .T. ) ;
#21120 = CARTESIAN_POINT ( 'NONE',  ( 12.69999999999999929, -3639.502500000000055, 2295.829799999999977 ) ) ;
#21121 = AXIS2_PLACEMENT_3D ( 'NONE', #8657, #1743, #21080 ) ;
#21122 = ORIENTED_EDGE ( 'NONE', *, *, #22453, .T. ) ;
#21123 = DIRECTION ( 'NONE',  ( 0.000000000000000000, 0.000000000000000000, 1.000000000000000000 ) ) ;
#21124 = CARTESIAN_POINT ( 'NONE',  ( 139.6999999999999886, -3579.494999999999891, 2246.630000000000109 ) ) ;
#21125 = MANIFOLD_SOLID_BREP ( 'SOLID2-16[1]', #139 ) ;
#21126 =( LENGTH_UNIT ( ) NAMED_UNIT ( * ) SI_UNIT ( .MILLI., .METRE. ) );
#21127 = DIRECTION ( 'NONE',  ( -2.324635735433000053E-14, 2.336881798971000105E-14, -1.000000000000000000 ) ) ;
#21128 = AXIS2_PLACEMENT_3D ( 'NONE', #2298, #12844, #12496 ) ;
#21129 = FACE_OUTER_BOUND ( 'NONE', #20924, .T. ) ;
#21130 = PERSON_AND_ORGANIZATION_ROLE ( 'design_supplier' ) ;
#21131 = DIRECTION ( 'NONE',  ( 0.000000000000000000, 0.000000000000000000, -1.000000000000000000 ) ) ;
#21132 = DIRECTION ( 'NONE',  ( 0.000000000000000000, 0.000000000000000000, -1.000000000000000000 ) ) ;
#21133 = CARTESIAN_POINT ( 'NONE',  ( 12.69999999999999929, -3585.210000000000036, 2268.705139999999574 ) ) ;
#21134 = CARTESIAN_POINT ( 'NONE',  ( 141.5613417780174927, -3657.352510518997406, 2246.797770067877991 ) ) ;
#21135 = EDGE_CURVE ( 'NONE', #22822, #13051, #2089, .T. ) ;
#21136 = ORIENTED_EDGE ( 'NONE', *, *, #7221, .T. ) ;
#21137 = TOROIDAL_SURFACE ( 'NONE', #18134, 5.588000000000000078, 0.7620000000000000107 ) ;
#21138 = EDGE_CURVE ( 'NONE', #20779, #17905, #11783, .T. ) ;
#21139 = CARTESIAN_POINT ( 'NONE',  ( 3.048000000000000043, -3544.061999999999898, 2228.849999999999909 ) ) ;
#21141 = EDGE_CURVE ( 'NONE', #7174, #17332, #20884, .T. ) ;
#21140 = AXIS2_PLACEMENT_3D ( 'NONE', #14317, #21458, #5410 ) ;
#21142 = ORIENTED_EDGE ( 'NONE', *, *, #4933, .F. ) ;
#21143 = AXIS2_PLACEMENT_3D ( 'NONE', #7088, #23120, #9190 ) ;
#21144 = ORIENTED_EDGE ( 'NONE', *, *, #14855, .T. ) ;
#21145 = ORIENTED_EDGE ( 'NONE', *, *, #4489, .F. ) ;
#21146 = CARTESIAN_POINT ( 'NONE',  ( 57.14999999999999858, -3695.699999999999818, 2247.392000000000280 ) ) ;
#21147 = ORIENTED_EDGE ( 'NONE', *, *, #3051, .F. ) ;
#21148 = ORIENTED_EDGE ( 'NONE', *, *, #1102, .T. ) ;
#21149 = CARTESIAN_POINT ( 'NONE',  ( 4.767653496878255126, -3543.397347668057137, 2259.817636094936915 ) ) ;
#21150 = DATE_TIME_ROLE ( 'classification_date' ) ;
#21151 = CARTESIAN_POINT ( 'NONE',  ( 12.69999999996000106, -3602.189899999999852, 2292.781800000000203 ) ) ;
#21152 = DIRECTION ( 'NONE',  ( -1.000000000000000000, 0.000000000000000000, 0.000000000000000000 ) ) ;
#21153 = VERTEX_POINT ( 'NONE', #9976 ) ;
#21154 = FACE_OUTER_BOUND ( 'NONE', #192, .T. ) ;
#21155 = FACE_BOUND ( 'NONE', #12131, .T. ) ;
#21156 = DIRECTION ( 'NONE',  ( -0.7071067811865975328, 0.000000000000000000, 0.7071067811864976127 ) ) ;
#21157 = CIRCLE ( 'NONE', #15175, 2.844799999998995244 ) ;
#21158 = VECTOR ( 'NONE', #10733, 1000.000000000000000 ) ;
#21159 = ORIENTED_EDGE ( 'NONE', *, *, #6869, .F. ) ;
#21160 = PERSON_AND_ORGANIZATION ( #5446, #1895 ) ;
#21161 = CIRCLE ( 'NONE', #16284, 3.606800000000000228 ) ;
#21162 = APPLICATION_CONTEXT ( 'configuration controlled 3d designs of mechanical parts and assemblies' ) ;
#21163 = CIRCLE ( 'NONE', #17786, 0.7619999999999294005 ) ;
#21164 = DIRECTION ( 'NONE',  ( -0.8660254037839826280, -0.5000000000007898127, 0.000000000000000000 ) ) ;
#21165 = CARTESIAN_POINT ( 'NONE',  ( 10.43004745555305846, -3581.209769231029895, 2248.995792276846714 ) ) ;
#21166 = CARTESIAN_POINT ( 'NONE',  ( 127.0000000000000000, -3568.700000000000273, 2239.009999999999764 ) ) ;
#21167 = ORIENTED_EDGE ( 'NONE', *, *, #19257, .T. ) ;
#21168 = DIRECTION ( 'NONE',  ( 0.000000000000000000, 0.000000000000000000, 1.000000000000000000 ) ) ;
#21169 = CIRCLE ( 'NONE', #7694, 3.606799999998994366 ) ;
#21170 = FACE_OUTER_BOUND ( 'NONE', #6528, .T. ) ;
#21171 = CARTESIAN_POINT ( 'NONE',  ( 145.1609999999999729, -3659.504999999999654, 2239.390999999999622 ) ) ;
#21172 = B_SPLINE_CURVE_WITH_KNOTS ( 'NONE', 3,
 ( #10332, #19242, #1181, #12091, #17588, #3179, #17475, #22748, #4943, #6605 ),
 .UNSPECIFIED., .F., .F.,
 ( 4, 2, 1, 1, 2, 4 ),
 ( 0.000000000000000000, 0.06249999999947680740, 0.1249999999989536148, 0.2500000000000294209, 0.5000000000000967004, 1.000000000000000000 ),
 .UNSPECIFIED. ) ;
#21173 = CARTESIAN_POINT ( 'NONE',  ( 12.69999999999999929, -3639.502500000000055, 2296.591799999999694 ) ) ;
#21174 = CIRCLE ( 'NONE', #10303, 1.269999999999882334 ) ;
#21175 = CARTESIAN_POINT ( 'NONE',  ( 10.87509742458831319, -3661.689672940328819, 2249.779197371474766 ) ) ;
#21176 = PRODUCT ( 'Screw 2', 'Screw 2', '', ( #15156 ) ) ;
#21177 = ADVANCED_FACE ( 'NONE', ( #22622 ), #14044, .T. ) ;
#21178 = EDGE_CURVE ( 'NONE', #2888, #23163, #6712, .T. ) ;
#21179 = DIRECTION ( 'NONE',  ( 0.000000000000000000, 0.000000000000000000, -1.000000000000000000 ) ) ;
#21180 = AXIS2_PLACEMENT_3D ( 'NONE', #15227, #22358, #17550 ) ;
#21181 = ORIENTED_EDGE ( 'NONE', *, *, #10817, .T. ) ;
#21182 = EDGE_CURVE ( 'NONE', #22614, #18910, #8224, .T. ) ;
#21183 = CARTESIAN_POINT ( 'NONE',  ( -5.588000000000000078, -3695.699999999999818, 2253.487999999999829 ) ) ;
#21184 = DIRECTION ( 'NONE',  ( 0.000000000000000000, 0.000000000000000000, -1.000000000000000000 ) ) ;
#21185 = DIRECTION ( 'NONE',  ( 1.000000000000000000, 0.000000000000000000, -1.224646799147353207E-16 ) ) ;
#21186 = CARTESIAN_POINT ( 'NONE',  ( 15.08810205602369514, -3657.959134956293383, 2249.218684437550110 ) ) ;
#21187 = CARTESIAN_POINT ( 'NONE',  ( 15.52167594717750809, -3579.072456535235233, 2250.236800948000109 ) ) ;
#21188 = VERTEX_POINT ( 'NONE', #8922 ) ;
#21189 = DIRECTION ( 'NONE',  ( -1.000000000000000000, -2.848935406719999894E-12, 0.000000000000000000 ) ) ;
#21190 = AXIS2_PLACEMENT_3D ( 'NONE', #4400, #753, #22421 ) ;
#21191 = DIRECTION ( 'NONE',  ( 0.000000000000000000, -1.000000000000000000, 1.319970543219000025E-14 ) ) ;
#21192 = VECTOR ( 'NONE', #12379, 1000.000000000000000 ) ;
#21193 = APPROVAL_STATUS ( 'not_yet_approved' ) ;
#21194 = EDGE_CURVE ( 'NONE', #13523, #16093, #17781, .T. ) ;
#21195 = LINE ( 'NONE', #19077, #4210 ) ;
#21196 = ADVANCED_FACE ( 'NONE', ( #5412 ), #14320, .T. ) ;
#21197 = DIRECTION ( 'NONE',  ( -1.000000000000000000, 0.000000000000000000, 0.000000000000000000 ) ) ;
#21198 = LINE ( 'NONE', #15570, #10699 ) ;
#21199 = CIRCLE ( 'NONE', #4725, 2.844799999999994444 ) ;
#21200 = DIRECTION ( 'NONE',  ( -1.000000000000000000, 0.000000000000000000, 0.000000000000000000 ) ) ;
#21201 = CARTESIAN_POINT ( 'NONE',  ( 17.49835313622208233, -3576.390213567464798, 2245.979654398315688 ) ) ;
#21202 = VECTOR ( 'NONE', #22143, 1000.000000000000000 ) ;
#21203 = CIRCLE ( 'NONE', #5870, 2.844799999999994444 ) ;
#21204 = FACE_OUTER_BOUND ( 'NONE', #16334, .T. ) ;
#21205 = ORIENTED_EDGE ( 'NONE', *, *, #21400, .T. ) ;
#21206 = CARTESIAN_POINT ( 'NONE',  ( 25.39999999999999858, -3670.300000000000182, 2260.600000000000364 ) ) ;
#21207 = ADVANCED_FACE ( 'NONE', ( #7062 ), #8804, .T. ) ;
#21208 = MANIFOLD_SOLID_BREP ( 'TORNILLO3[1]', #13596 ) ;
#21209 = DIRECTION ( 'NONE',  ( 0.000000000000000000, 0.000000000000000000, -1.000000000000000000 ) ) ;
#21210 = ORIENTED_EDGE ( 'NONE', *, *, #14817, .F. ) ;
#21211 = CARTESIAN_POINT ( 'NONE',  ( 21.79320000000099711, -3670.300000000000182, 2239.009999999999764 ) ) ;
#21212 = VECTOR ( 'NONE', #16107, 1000.000000000000000 ) ;
#21213 = VERTEX_POINT ( 'NONE', #7713 ) ;
#21214 = CARTESIAN_POINT ( 'NONE',  ( 134.2546079315347356, -3581.231065619790115, 2245.814675045431159 ) ) ;
#21215 = ORIENTED_EDGE ( 'NONE', *, *, #11232, .T. ) ;
#21216 = ORIENTED_EDGE ( 'NONE', *, *, #9360, .F. ) ;
#21217 = FACE_OUTER_BOUND ( 'NONE', #22458, .T. ) ;
#21218 = APPROVAL_DATE_TIME ( #9342, #12657 ) ;
#21219 = DIRECTION ( 'NONE',  ( 0.6887494619147658259, 0.000000000000000000, -0.7249994335943447110 ) ) ;
#21220 = ORIENTED_EDGE ( 'NONE', *, *, #22020, .F. ) ;
#21221 = DIRECTION ( 'NONE',  ( 0.000000000000000000, -1.000000000000000000, 0.000000000000000000 ) ) ;
#21222 = COORDINATED_UNIVERSAL_TIME_OFFSET ( 0, 0, .AHEAD. ) ;
#21223 = DIRECTION ( 'NONE',  ( -1.000000000000000000, 0.000000000000000000, 0.000000000000000000 ) ) ;
#21224 = CARTESIAN_POINT ( 'NONE',  ( 15.01285743453679267, -3581.153169946162961, 2249.079238002240345 ) ) ;
#21225 = VECTOR ( 'NONE', #11719, 1000.000000000000000 ) ;
#21226 = CARTESIAN_POINT ( 'NONE',  ( 17.78000000000000114, -3579.494999999999891, 2245.359999999999673 ) ) ;
#21227 = DIRECTION ( 'NONE',  ( 0.000000000000000000, -1.000000000000000000, 0.000000000000000000 ) ) ;
#21228 = AXIS2_PLACEMENT_3D ( 'NONE', #13623, #17131, #11740 ) ;
#21229 = DIRECTION ( 'NONE',  ( 0.000000000000000000, 0.000000000000000000, 1.000000000000000000 ) ) ;
#21230 = EDGE_LOOP ( 'NONE', ( #18024, #5857, #11942, #10425, #5027 ) ) ;
#21231 = CARTESIAN_POINT ( 'NONE',  ( 79.80679999999999552, -3568.700000000000273, 2239.009999999999764 ) ) ;
#21232 = AXIS2_PLACEMENT_3D ( 'NONE', #1589, #10383, #21404 ) ;
#21233 = DIRECTION ( 'NONE',  ( 1.000000000000000000, 0.000000000000000000, 0.000000000000000000 ) ) ;
#21234 = ORIENTED_EDGE ( 'NONE', *, *, #21561, .T. ) ;
#21235 = CARTESIAN_POINT ( 'NONE',  ( 15.03168679710029743, -3658.158799999889197, 2239.391000000000076 ) ) ;
#21236 = PRODUCT_RELATED_PRODUCT_CATEGORY ( 'detail', '', ( #7149 ) ) ;
#21237 = LINE ( 'NONE', #4939, #3192 ) ;
#21238 = ORIENTED_EDGE ( 'NONE', *, *, #10833, .F. ) ;
#21239 = ORIENTED_EDGE ( 'NONE', *, *, #81, .F. ) ;
#21240 = DIRECTION ( 'NONE',  ( 0.000000000000000000, 0.000000000000000000, -1.000000000000000000 ) ) ;
#21241 = CARTESIAN_POINT ( 'NONE',  ( 139.6999999999999886, -3579.494999999999891, 2239.771999999999935 ) ) ;
#21242 = ORIENTED_EDGE ( 'NONE', *, *, #14557, .T. ) ;
#21243 = CIRCLE ( 'NONE', #6661, 0.7619999999999294005 ) ;
#21244 = CARTESIAN_POINT ( 'NONE',  ( -0.7620000000000000107, -3544.061999999999898, 2253.487999999999829 ) ) ;
#21245 = CARTESIAN_POINT ( 'NONE',  ( 15.47880416110802670, -3660.114175108592917, 2250.236712862199965 ) ) ;
#21246 = EDGE_CURVE ( 'NONE', #11590, #15211, #7679, .T. ) ;
#21247 = CARTESIAN_POINT ( 'NONE',  ( 136.8551999999999964, -3579.495007806000103, 2250.165025852999861 ) ) ;
#21248 = CALENDAR_DATE ( 2026, 26, 10 ) ;
#21249 = ADVANCED_FACE ( 'NONE', ( #5856 ), #5295, .T. ) ;
#21250 = AXIS2_PLACEMENT_3D ( 'NONE', #16261, #3259, #3718 ) ;
#21251 = AXIS2_PLACEMENT_3D ( 'NONE', #20624, #15710, #940 ) ;
#21252 = DIRECTION ( 'NONE',  ( 1.000000000000000000, -1.165588477296748772E-12, 0.000000000000000000 ) ) ;
#21253 = CARTESIAN_POINT ( 'NONE',  ( 139.6999999999999886, -3656.329999999999472, 2245.359999999999673 ) ) ;
#21254 = CARTESIAN_POINT ( 'NONE',  ( 137.5852380282969136, -3657.602178072644620, 2248.677473072372322 ) ) ;
#21255 = ORIENTED_EDGE ( 'NONE', *, *, #12439, .T. ) ;
#21256 = DIRECTION ( 'NONE',  ( 0.000000000000000000, 1.000000000000000000, 0.000000000000000000 ) ) ;
#21257 = CIRCLE ( 'NONE', #15264, 5.080000000000000959 ) ;
#21258 = ORIENTED_EDGE ( 'NONE', *, *, #9365, .T. ) ;
#21259 = VERTEX_POINT ( 'NONE', #4191 ) ;
#21260 = ORIENTED_EDGE ( 'NONE', *, *, #3256, .T. ) ;
#21261 = CIRCLE ( 'NONE', #1411, 0.7619999999999294005 ) ;
#21262 = APPROVAL ( #11430, 'UNSPECIFIED' ) ;
#21263 = LINE ( 'NONE', #19495, #7720 ) ;
#21264 = ORIENTED_EDGE ( 'NONE', *, *, #9516, .F. ) ;
#21265 = ORIENTED_EDGE ( 'NONE', *, *, #14297, .F. ) ;
#21266 = CARTESIAN_POINT ( 'NONE',  ( 139.6999999999999886, -3662.197400000000016, 2242.820000000000164 ) ) ;
#21267 = DIRECTION ( 'NONE',  ( 0.000000000000000000, -1.000000000000000000, 0.000000000000000000 ) ) ;
#21268 = CARTESIAN_POINT ( 'NONE',  ( 18.16100000000000136, -3659.504999999999654, 2239.391000000000076 ) ) ;
#21269 = ORIENTED_EDGE ( 'NONE', *, *, #20870, .F. ) ;
#21270 = DIRECTION ( 'NONE',  ( -1.000000000000000000, 0.000000000000000000, 0.000000000000000000 ) ) ;
#21271 = ORIENTED_EDGE ( 'NONE', *, *, #7543, .F. ) ;
#21272 = ADVANCED_FACE ( 'NONE', ( #11335 ), #5965, .T. ) ;
#21273 = CARTESIAN_POINT ( 'NONE',  ( 12.69999999999999929, -3579.494999999999891, 2239.391000000000076 ) ) ;
#21274 = CARTESIAN_POINT ( 'NONE',  ( 12.69999999999999929, -3599.497499999999945, 2290.622800000000097 ) ) ;
#21275 = DIRECTION ( 'NONE',  ( 2.330758767201999921E-14, 1.000000000000000000, -5.460979050843892707E-28 ) ) ;
#21276 = ADVANCED_FACE ( 'NONE', ( #14754 ), #11224, .F. ) ;
#21277 = ORIENTED_EDGE ( 'NONE', *, *, #7436, .F. ) ;
#21278 = PERSON_AND_ORGANIZATION ( #5446, #1895 ) ;
#21279 = EDGE_CURVE ( 'NONE', #16839, #8573, #17799, .T. ) ;
#21280 = AXIS2_PLACEMENT_3D ( 'NONE', #9053, #20075, #14681 ) ;
#21281 = EDGE_LOOP ( 'NONE', ( #2637, #1898, #10541, #1136 ) ) ;
#21282 = DIRECTION ( 'NONE',  ( 0.000000000000000000, 0.000000000000000000, -1.000000000000000000 ) ) ;
#21283 = CARTESIAN_POINT ( 'NONE',  ( 10.29510451277807093, -3581.014576728029624, 2249.249714666130330 ) ) ;
#21284 = MANIFOLD_SOLID_BREP ( 'SOLID21[1]', #867 ) ;
#21285 = CARTESIAN_POINT ( 'NONE',  ( 151.1299999999999955, -3578.860000000000127, 2247.392000000000280 ) ) ;
#21286 = ADVANCED_FACE ( 'NONE', ( #12437 ), #18370, .T. ) ;
#21287 = EDGE_LOOP ( 'NONE', ( #2598, #15199, #21914 ) ) ;
#21288 = FACE_BOUND ( 'NONE', #13387, .T. ) ;
#21289 = EDGE_CURVE ( 'NONE', #18476, #2750, #450, .T. ) ;
#21290 = CYLINDRICAL_SURFACE ( 'NONE', #5416, 3.175000000000149925 ) ;
#21291 = CARTESIAN_POINT ( 'NONE',  ( 15.41268679716529455, -3581.061170452570423, 2239.009999999999764 ) ) ;
#21292 = CARTESIAN_POINT ( 'NONE',  ( 142.5447999999989861, -3659.504999999999654, 2272.030000000000200 ) ) ;
#21293 = CARTESIAN_POINT ( 'NONE',  ( 10.67302639621317795, -3661.501522125889096, 2249.890123210526326 ) ) ;
#21294 = ORIENTED_EDGE ( 'NONE', *, *, #17018, .F. ) ;
#21295 = CARTESIAN_POINT ( 'NONE',  ( 15.54478936534684941, -3659.505023738319323, 2250.165136749944850 ) ) ;
#21296 = VERTEX_POINT ( 'NONE', #9585 ) ;
#21297 = CARTESIAN_POINT ( 'NONE',  ( 137.3683132028983493, -3578.148799999801213, 2239.167815367371077 ) ) ;
#21298 = DIRECTION ( 'NONE',  ( 0.000000000000000000, 1.000000000000000000, 0.000000000000000000 ) ) ;
#21299 = LINE ( 'NONE', #7011, #1853 ) ;
#21300 = CARTESIAN_POINT ( 'NONE',  ( 15.34531583769129526, -3658.458524271727129, 2249.686710455694993 ) ) ;
#21301 = CARTESIAN_POINT ( 'NONE',  ( 137.0372536546044842, -3695.258941568228238, 2255.466568422051296 ) ) ;
#21302 = ORIENTED_EDGE ( 'NONE', *, *, #17471, .F. ) ;
#21303 = DIRECTION ( 'NONE',  ( 1.073225997510925892E-13, 0.000000000000000000, 1.000000000000000000 ) ) ;
#21304 = ORIENTED_EDGE ( 'NONE', *, *, #18994, .T. ) ;
#21305 = EDGE_CURVE ( 'NONE', #6861, #21259, #10695, .T. ) ;
#21306 = FACE_OUTER_BOUND ( 'NONE', #18215, .T. ) ;
#21307 = CYLINDRICAL_SURFACE ( 'NONE', #15635, 3.175000000000149925 ) ;
#21308 = PERSON_AND_ORGANIZATION ( #6273, #9025 ) ;
#21309 = ADVANCED_FACE ( 'NONE', ( #3521 ), #10678, .F. ) ;
#21310 = CARTESIAN_POINT ( 'NONE',  ( 18.01287425285000410, -3657.399152860999493, 2246.630000000000109 ) ) ;
#21311 = EDGE_CURVE ( 'NONE', #1860, #15900, #7594, .T. ) ;
#21312 = FACE_OUTER_BOUND ( 'NONE', #127, .T. ) ;
#21313 = CARTESIAN_POINT ( 'NONE',  ( -0.7620000000000000107, -3578.860000000000127, 2247.392000000000280 ) ) ;
#21314 = CIRCLE ( 'NONE', #1081, 0.7620000000000000107 ) ;
#21315 = DIRECTION ( 'NONE',  ( 0.000000000000000000, 0.000000000000000000, 1.000000000000000000 ) ) ;
#21316 = CARTESIAN_POINT ( 'NONE',  ( -5.588000000000000078, -3695.699999999999818, 2253.487999999999829 ) ) ;
#21317 = CARTESIAN_POINT ( 'NONE',  ( 21.79320000000099711, -3619.500000000000000, 2239.771999999999935 ) ) ;
#21318 = EDGE_CURVE ( 'NONE', #1510, #18991, #17813, .T. ) ;
#21319 = ORIENTED_EDGE ( 'NONE', *, *, #6012, .F. ) ;
#21320 = PLANE ( 'NONE',  #15182 ) ;
#21321 = DIRECTION ( 'NONE',  ( -0.8660254037819670181, -0.5000000000042810200, 0.000000000000000000 ) ) ;
#21322 = ORIENTED_EDGE ( 'NONE', *, *, #818, .T. ) ;
#21323 = CARTESIAN_POINT ( 'NONE',  ( 12.69999999999999929, -3639.502500000000055, 2290.622800000000097 ) ) ;
#21324 = EDGE_CURVE ( 'NONE', #10158, #6778, #22280, .T. ) ;
#21325 = ORIENTED_EDGE ( 'NONE', *, *, #746, .F. ) ;
#21326 = CARTESIAN_POINT ( 'NONE',  ( 64.76999999999999602, -3568.700000000000273, 2292.057900000000245 ) ) ;
#21327 = AXIS2_PLACEMENT_3D ( 'NONE', #3326, #12247, #17742 ) ;
#21328 = ORIENTED_EDGE ( 'NONE', *, *, #5737, .T. ) ;
#21329 = ORIENTED_EDGE ( 'NONE', *, *, #20614, .F. ) ;
#21330 = CARTESIAN_POINT ( 'NONE',  ( 12.69999999999999929, -3639.502500000000055, 2264.841800000000148 ) ) ;
#21331 = ORIENTED_EDGE ( 'NONE', *, *, #12593, .F. ) ;
#21332 = DIRECTION ( 'NONE',  ( -1.000000000000000000, 2.331176954593508450E-12, 0.000000000000000000 ) ) ;
#21333 = COORDINATED_UNIVERSAL_TIME_OFFSET ( 0, 0, .AHEAD. ) ;
#21334 = EDGE_CURVE ( 'NONE', #21632, #17332, #18643, .T. ) ;
#21335 = CYLINDRICAL_SURFACE ( 'NONE', #22430, 1.269999999999882334 ) ;
#21336 = CARTESIAN_POINT ( 'NONE',  ( 14.85086632574098964, -3581.357178777328954, 2248.755707450937734 ) ) ;
#21337 = AXIS2_PLACEMENT_3D ( 'NONE', #10779, #5278, #1872 ) ;
#21338 = DIRECTION ( 'NONE',  ( -1.000000000000000000, 0.000000000000000000, 0.000000000000000000 ) ) ;
#21339 = FACE_OUTER_BOUND ( 'NONE', #2621, .T. ) ;
#21340 = APPROVAL_PERSON_ORGANIZATION ( #6488, #18651, #3423 ) ;
#21341 = EDGE_LOOP ( 'NONE', ( #707, #6389, #2604, #10086 ) ) ;
#21342 = AXIS2_PLACEMENT_3D ( 'NONE', #20175, #6345, #8100 ) ;
#21343 = SPHERICAL_SURFACE ( 'NONE', #4326, 1.270000000000000018 ) ;
#21344 = FACE_OUTER_BOUND ( 'NONE', #11178, .T. ) ;
#21345 = ORIENTED_EDGE ( 'NONE', *, *, #577, .T. ) ;
#21346 = DIRECTION ( 'NONE',  ( -2.324635735433000053E-14, 0.000000000000000000, -1.000000000000000000 ) ) ;
#21347 = DIRECTION ( 'NONE',  ( 0.000000000000000000, 0.000000000000000000, -1.000000000000000000 ) ) ;
#21348 = SHAPE_REPRESENTATION ( 'Screw 5', ( #5611 ), #13859 ) ;
#21349 = EDGE_CURVE ( 'NONE', #1150, #523, #11668, .T. ) ;
#21350 = CARTESIAN_POINT ( 'NONE',  ( 20.31206600733000300, -3544.241663918999620, 2260.533847755999886 ) ) ;
#21351 = VERTEX_POINT ( 'NONE', #3006 ) ;
#21352 = CARTESIAN_POINT ( 'NONE',  ( 20.32000000000000028, -3670.300000000000182, 2289.213099999999940 ) ) ;
#21353 = CARTESIAN_POINT ( 'NONE',  ( 15.41268679728733915, -3657.938829547220848, 2239.009999999999764 ) ) ;
#21354 = AXIS2_PLACEMENT_3D ( 'NONE', #6901, #1738, #3484 ) ;
#21355 = ORIENTED_EDGE ( 'NONE', *, *, #21839, .T. ) ;
#21356 = CARTESIAN_POINT ( 'NONE',  ( 9.855200000000998273, -3659.504999999999654, 2256.063560000000052 ) ) ;
#21357 = CARTESIAN_POINT ( 'NONE',  ( 12.07314413848000001, -3642.283404631000394, 2279.801389126999766 ) ) ;
#21358 = APPLIED_APPROVAL_ASSIGNMENT ( #13928, ( #28 ) ) ;
#21359 = APPROVAL_PERSON_ORGANIZATION ( #16224, #16798, #17746 ) ;
#21360 = APPLICATION_PROTOCOL_DEFINITION ( 'international standard', 'automotive_design', 2000, #21162 ) ;
#21361 = VERTEX_POINT ( 'NONE', #2551 ) ;
#21362 = PLANE ( 'NONE',  #23100 ) ;
#21363 = CARTESIAN_POINT ( 'NONE',  ( 20.32000000000000028, -3568.700000000000273, 2289.213099999999940 ) ) ;
#21364 = DIRECTION ( 'NONE',  ( -1.000000000000000000, 0.000000000000000000, 0.000000000000000000 ) ) ;
#21365 = APPLIED_PERSON_AND_ORGANIZATION_ASSIGNMENT ( #22810, #3253, ( #12016 ) ) ;
#21366 = DIRECTION ( 'NONE',  ( 0.000000000000000000, -1.000000000000000000, 0.000000000000000000 ) ) ;
#21367 = VERTEX_POINT ( 'NONE', #2894 ) ;
#21368 = DIRECTION ( 'NONE',  ( 1.000000000000000000, 4.457711412217000029E-12, 2.901972884401000201E-13 ) ) ;
#21369 = ORIENTED_EDGE ( 'NONE', *, *, #2078, .T. ) ;
#21370 = ORIENTED_EDGE ( 'NONE', *, *, #3846, .T. ) ;
#21371 = ORGANIZATION ( 'NAUO-ORG11', 'UNSPECIFIED', 'UNSPECIFIED' ) ;
#21372 = APPLIED_APPROVAL_ASSIGNMENT ( #1616, ( #11226 ) ) ;
#21373 = ORIENTED_EDGE ( 'NONE', *, *, #13086, .F. ) ;
#21374 = CARTESIAN_POINT ( 'NONE',  ( -12.31900000000000084, -3657.790744320999693, 2246.035656601000028 ) ) ;
#21375 = ORIENTED_EDGE ( 'NONE', *, *, #19816, .F. ) ;
#21376 = EDGE_LOOP ( 'NONE', ( #11448, #11254, #15300, #4099 ) ) ;
#21377 = CARTESIAN_POINT ( 'NONE',  ( -6.730999999999999872, -3660.140000000000327, 2247.392000000000280 ) ) ;
#21378 = DATE_TIME_ROLE ( 'classification_date' ) ;
#21379 = DIRECTION ( 'NONE',  ( 1.000000000000000000, 0.000000000000000000, 0.000000000000000000 ) ) ;
#21380 = ADVANCED_BREP_SHAPE_REPRESENTATION ( '', ( #21125, #5611 ), #2239 ) ;
#21381 = FACE_OUTER_BOUND ( 'NONE', #18280, .T. ) ;
#21382 = VERTEX_POINT ( 'NONE', #13677 ) ;
#21383 = CIRCLE ( 'NONE', #11273, 1.240967364599221412 ) ;
#21384 = DIRECTION ( 'NONE',  ( -2.185478394939000111E-13, 1.295098308111999954E-13, -1.000000000000000000 ) ) ;
#21385 = DIRECTION ( 'NONE',  ( 0.000000000000000000, 0.000000000000000000, -1.000000000000000000 ) ) ;
#21386 = DIRECTION ( 'NONE',  ( 1.000000000000000000, 0.000000000000000000, 0.000000000000000000 ) ) ;
#21387 = DIRECTION ( 'NONE',  ( 1.073225997510925892E-13, 0.000000000000000000, 1.000000000000000000 ) ) ;
#21388 = ORIENTED_EDGE ( 'NONE', *, *, #18364, .T. ) ;
#21389 = APPROVAL_ROLE ( '' ) ;
#21390 = CYLINDRICAL_SURFACE ( 'NONE', #16535, 1.269999999999898099 ) ;
#21391 = APPROVAL_PERSON_ORGANIZATION ( #1919, #14062, #5325 ) ;
#21392 = APPLIED_PERSON_AND_ORGANIZATION_ASSIGNMENT ( #3187, #6723, ( #19099 ) ) ;
#21393 = DIRECTION ( 'NONE',  ( 0.000000000000000000, -1.000000000000000000, 0.000000000000000000 ) ) ;
#21394 = CARTESIAN_POINT ( 'NONE',  ( 18.41499999999999915, -3639.502500000000055, 2288.971800000000258 ) ) ;
#21395 = VERTEX_POINT ( 'NONE', #8175 ) ;
#21396 = AXIS2_PLACEMENT_3D ( 'NONE', #11319, #18469, #14960 ) ;
#21397 = FACE_BOUND ( 'NONE', #18473, .T. ) ;
#21398 = AXIS2_PLACEMENT_3D ( 'NONE', #13616, #1070, #20524 ) ;
#21399 = EDGE_CURVE ( 'NONE', #13234, #17172, #21169, .T. ) ;
#21400 = EDGE_CURVE ( 'NONE', #2236, #671, #4768, .T. ) ;
#21401 = CARTESIAN_POINT ( 'NONE',  ( 12.69999999999999929, -3599.497499999999945, 2290.241799999999785 ) ) ;
#21402 = CARTESIAN_POINT ( 'NONE',  ( 15.03168679710930178, -3580.841200000109893, 2239.391000000000076 ) ) ;
#21403 = B_SPLINE_CURVE_WITH_KNOTS ( 'NONE', 3,
 ( #13196, #9350, #4069, #16487, #5731, #11439, #20353, #3955, #13089, #20240, #18591, #9238, #11324, #18474, #16717, #16824, #669 ),
 .UNSPECIFIED., .F., .F.,
 ( 4, 2, 2, 1, 2, 2, 2, 2, 4 ),
 ( 0.000000000000000000, 0.1249999999998916422, 0.1875000000000623945, 0.2187500000002796374, 0.2343750000001848244, 0.2500000000000900391, 0.5000000000000599520, 0.7500000000000299760, 1.000000000000000000 ),
 .UNSPECIFIED. ) ;
#21404 = DIRECTION ( 'NONE',  ( 0.000000000000000000, 0.000000000000000000, 1.000000000000000000 ) ) ;
#21405 = DIRECTION ( 'NONE',  ( 1.000000000000000000, 0.000000000000000000, 0.000000000000000000 ) ) ;
#21406 = EDGE_CURVE ( 'NONE', #12409, #22852, #15560, .T. ) ;
#21407 = DIRECTION ( 'NONE',  ( -1.000000000000000000, 0.000000000000000000, -3.680805717774999826E-13 ) ) ;
#21408 = VERTEX_POINT ( 'NONE', #8405 ) ;
#21409 = DIRECTION ( 'NONE',  ( -1.000000000000000000, 0.000000000000000000, 0.000000000000000000 ) ) ;
#21410 = DIRECTION ( 'NONE',  ( -1.000000000000000000, 0.000000000000000000, 0.000000000000000000 ) ) ;
#21411 = LINE ( 'NONE', #7349, #19059 ) ;
#21412 = CARTESIAN_POINT ( 'NONE',  ( 14.62318399493629784, -3657.408672365483653, 2248.187748315331646 ) ) ;
#21413 = ADVANCED_FACE ( 'NONE', ( #22689 ), #18827, .T. ) ;
#21414 = CARTESIAN_POINT ( 'NONE',  ( 136.8552720942020073, -3695.594480551561446, 2255.010851275907498 ) ) ;
#21415 = AXIS2_PLACEMENT_3D ( 'NONE', #4038, #18327, #9429 ) ;
#21416 = CARTESIAN_POINT ( 'NONE',  ( 10.10523630290581565, -3578.289363367462556, 2250.192408352016173 ) ) ;
#21417 = EDGE_LOOP ( 'NONE', ( #1021, #18881, #88, #7828, #20000, #20751 ) ) ;
#21418 = AXIS2_PLACEMENT_3D ( 'NONE', #2474, #4562, #17098 ) ;
#21419 = CARTESIAN_POINT ( 'NONE',  ( 12.70000000003999929, -3582.187399999999798, 2242.820000000000164 ) ) ;
#21420 = ADVANCED_FACE ( 'NONE', ( #15436 ), #1011, .T. ) ;
#21421 = COORDINATED_UNIVERSAL_TIME_OFFSET ( 0, 0, .AHEAD. ) ;
#21422 = FACE_OUTER_BOUND ( 'NONE', #21816, .T. ) ;
#21423 = CARTESIAN_POINT ( 'NONE',  ( 12.69999999999999929, -3656.660200000000259, 2257.592639999999847 ) ) ;
#21424 = CARTESIAN_POINT ( 'NONE',  ( 12.69999999999999929, -3639.502500000000055, 2290.622800000000097 ) ) ;
#21425 = DIRECTION ( 'NONE',  ( 0.000000000000000000, 0.000000000000000000, -1.000000000000000000 ) ) ;
#21426 = AXIS2_PLACEMENT_3D ( 'NONE', #12281, #23042, #10515 ) ;
#21427 = ORIENTED_EDGE ( 'NONE', *, *, #5698, .F. ) ;
#21428 = PLANE ( 'NONE',  #162 ) ;
#21429 = ORIENTED_EDGE ( 'NONE', *, *, #7092, .F. ) ;
#21430 = VECTOR ( 'NONE', #6551, 1000.000000000000000 ) ;
#21431 = DIRECTION ( 'NONE',  ( 0.000000000000000000, 0.000000000000000000, 1.000000000000000000 ) ) ;
#21432 = ADVANCED_FACE ( 'NONE', ( #11452, #781, #7945 ), #22218, .F. ) ;
#21433 = AXIS2_PLACEMENT_3D ( 'NONE', #11338, #20583, #4534 ) ;
#21434 = CARTESIAN_POINT ( 'NONE',  ( 15.03168679714000078, -3600.843699999999899, 2296.210799999999836 ) ) ;
#21435 = ORIENTED_EDGE ( 'NONE', *, *, #3000, .F. ) ;
#21436 = CARTESIAN_POINT ( 'NONE',  ( 12.69999999999999929, -3659.504999999999654, 2272.030000000000200 ) ) ;
#21437 = ORIENTED_EDGE ( 'NONE', *, *, #14118, .T. ) ;
#21438 = CARTESIAN_POINT ( 'NONE',  ( 142.2881911273701689, -3694.976217802131487, 2255.653223149227415 ) ) ;
#21439 = FACE_OUTER_BOUND ( 'NONE', #22801, .T. ) ;
#21440 = VECTOR ( 'NONE', #13061, 1000.000000000000000 ) ;
#21441 = ORIENTED_EDGE ( 'NONE', *, *, #988, .F. ) ;
#21442 = EDGE_LOOP ( 'NONE', ( #11408, #5619, #2264, #14004 ) ) ;
#21443 = CARTESIAN_POINT ( 'NONE',  ( 137.2439122574247108, -3580.930587627222394, 2249.343187823710650 ) ) ;
#21444 = EDGE_LOOP ( 'NONE', ( #8698, #9307 ) ) ;
#21446 = CARTESIAN_POINT ( 'NONE',  ( 9.525000000260952504, -3695.384369265494115, 2281.351799999999912 ) ) ;
#21445 = CIRCLE ( 'NONE', #20673, 3.606799999999993567 ) ;
#21447 = APPROVAL_STATUS ( 'not_yet_approved' ) ;
#21448 = VECTOR ( 'NONE', #11312, 1000.000000000000000 ) ;
#21449 = CARTESIAN_POINT ( 'NONE',  ( 12.69999999999999929, -3659.504999999999654, 2255.774000000000342 ) ) ;
#21450 = CARTESIAN_POINT ( 'NONE',  ( 0.000000000000000000, -3578.860000000000127, 2247.392000000000280 ) ) ;
#21451 = FACE_OUTER_BOUND ( 'NONE', #8724, .T. ) ;
#21452 = DIRECTION ( 'NONE',  ( 0.000000000000000000, -1.000000000000000000, 0.000000000000000000 ) ) ;
#21453 = CARTESIAN_POINT ( 'NONE',  ( 1.270000000000000018, -3578.860000000000127, 2247.392000000000280 ) ) ;
#21454 = ORIENTED_EDGE ( 'NONE', *, *, #3930, .T. ) ;
#21455 = CARTESIAN_POINT ( 'NONE',  ( 134.0275598363577103, -3578.798113836681750, 2244.547775376694972 ) ) ;
#21456 = DIRECTION ( 'NONE',  ( 0.000000000000000000, 0.000000000000000000, 1.000000000000000000 ) ) ;
#21457 = ORIENTED_EDGE ( 'NONE', *, *, #7657, .F. ) ;
#21458 = DIRECTION ( 'NONE',  ( -3.194481088215918719E-14, -0.5000000000040877302, -0.8660254037820785955 ) ) ;
#21459 = CARTESIAN_POINT ( 'NONE',  ( 139.6999999999999886, -3659.504999999999654, 2239.391000000000076 ) ) ;
#21460 = AXIS2_PLACEMENT_3D ( 'NONE', #14241, #17508, #21386 ) ;
#21461 = ADVANCED_FACE ( 'NONE', ( #11560 ), #18706, .T. ) ;
#21462 = CIRCLE ( 'NONE', #16225, 3.175000000000149925 ) ;
#21463 = EDGE_CURVE ( 'NONE', #6658, #1958, #15207, .T. ) ;
#21464 = DIRECTION ( 'NONE',  ( 2.150065550568999996E-13, 0.000000000000000000, -1.000000000000000000 ) ) ;
#21465 = ORIENTED_EDGE ( 'NONE', *, *, #19286, .F. ) ;
#21466 = ADVANCED_FACE ( 'NONE', ( #4531 ), #15672, .T. ) ;
#21467 = CARTESIAN_POINT ( 'NONE',  ( 29.00679999999900005, -3619.500000000000000, 2259.837999999999738 ) ) ;
#21468 = FACE_OUTER_BOUND ( 'NONE', #1933, .T. ) ;
#21469 = ORIENTED_EDGE ( 'NONE', *, *, #12816, .F. ) ;
#21470 = DIRECTION ( 'NONE',  ( 0.000000000000000000, 0.000000000000000000, 1.000000000000000000 ) ) ;
#21471 = DIRECTION ( 'NONE',  ( 0.000000000000000000, 0.000000000000000000, -1.000000000000000000 ) ) ;
#21472 = MANIFOLD_SOLID_BREP ( 'SOLID2-14[1]', #9838 ) ;
#21473 = DIRECTION ( 'NONE',  ( -0.000000000000000000, 1.000000000000000000, 0.000000000000000000 ) ) ;
#21474 = ADVANCED_FACE ( 'NONE', ( #17530 ), #9210, .T. ) ;
#21475 = CARTESIAN_POINT ( 'NONE',  ( 19.05000000000000071, -3576.955000000000382, 2247.392000000000280 ) ) ;
#21476 = VECTOR ( 'NONE', #17664, 1000.000000000000000 ) ;
#21477 = CALENDAR_DATE ( 2026, 26, 10 ) ;
#21478 = EDGE_LOOP ( 'NONE', ( #8737, #20481, #20306, #18565 ) ) ;
#21479 = DIRECTION ( 'NONE',  ( -2.324635735433000053E-14, 0.000000000000000000, -1.000000000000000000 ) ) ;
#21480 = CARTESIAN_POINT ( 'NONE',  ( -8.890000000008001280, -3661.486200000000281, 2249.723686796999573 ) ) ;
#21481 = ORIENTED_EDGE ( 'NONE', *, *, #14817, .T. ) ;
#21482 = DIRECTION ( 'NONE',  ( -1.000000000000000000, 0.000000000000000000, 0.000000000000000000 ) ) ;
#21483 = EDGE_CURVE ( 'NONE', #22588, #13787, #14454, .T. ) ;
#21484 = CARTESIAN_POINT ( 'NONE',  ( 137.2895610191548599, -3657.994247822125999, 2249.259792710935926 ) ) ;
#21485 = EDGE_CURVE ( 'NONE', #18910, #14398, #8634, .T. ) ;
#21486 = ORIENTED_EDGE ( 'NONE', *, *, #13517, .F. ) ;
#21487 =( BOUNDED_CURVE ( )  B_SPLINE_CURVE ( 3, ( #9492, #7851, #16630, #588 ),
 .UNSPECIFIED., .F., .F. ) 
 B_SPLINE_CURVE_WITH_KNOTS ( ( 4, 4 ),
 ( 1.570796326625032657, 3.141592653589783346 ),
 .UNSPECIFIED. ) 
 CURVE ( )  GEOMETRIC_REPRESENTATION_ITEM ( )  RATIONAL_B_SPLINE_CURVE ( ( 1.000000000000000000, 0.8047378540843299621, 0.8047378540843299621, 1.000000000000000000 ) ) 
 REPRESENTATION_ITEM ( '' )  );
#21488 = CARTESIAN_POINT ( 'NONE',  ( 151.4000000000000057, -3695.699999999999818, 2295.829799999999977 ) ) ;
#21489 = ORIENTED_EDGE ( 'NONE', *, *, #18439, .F. ) ;
#21490 = VERTEX_POINT ( 'NONE', #5358 ) ;
#21491 = ORIENTED_EDGE ( 'NONE', *, *, #13378, .F. ) ;
#21492 = AXIS2_PLACEMENT_3D ( 'NONE', #10527, #17788, #3372 ) ;
#21493 = DIRECTION ( 'NONE',  ( 0.000000000000000000, -1.000000000000000000, 0.000000000000000000 ) ) ;
#21494 = AXIS2_PLACEMENT_3D ( 'NONE', #18001, #1950, #19882 ) ;
#21495 = ORIENTED_EDGE ( 'NONE', *, *, #1034, .T. ) ;
#21496 = ORIENTED_EDGE ( 'NONE', *, *, #20599, .T. ) ;
#21497 = FACE_OUTER_BOUND ( 'NONE', #13683, .T. ) ;
#21498 = APPROVAL_DATE_TIME ( #14000, #15483 ) ;
#21499 = DIRECTION ( 'NONE',  ( 0.000000000000000000, 0.000000000000000000, -1.000000000000000000 ) ) ;
#21500 = CARTESIAN_POINT ( 'NONE',  ( 12.69999999999999929, -3653.027999999999793, 2268.705139999999574 ) ) ;
#21501 = ORIENTED_EDGE ( 'NONE', *, *, #402, .F. ) ;
#21502 = DIRECTION ( 'NONE',  ( 0.000000000000000000, -0.5000000000005969669, 0.8660254037840939834 ) ) ;
#21503 = DIRECTION ( 'NONE',  ( 1.000000000000000000, 0.000000000000000000, 0.000000000000000000 ) ) ;
#21504 = DIRECTION ( 'NONE',  ( -2.343004830739999973E-14, -1.784212334590129905E-30, -1.000000000000000000 ) ) ;
#21505 = CARTESIAN_POINT ( 'NONE',  ( 12.69999999999999929, -3639.502500000000055, 2296.210799999999836 ) ) ;
#21506 = PERSON_AND_ORGANIZATION_ROLE ( 'classification_officer' ) ;
#21507 = ORIENTED_EDGE ( 'NONE', *, *, #9652, .T. ) ;
#21508 = CARTESIAN_POINT ( 'NONE',  ( 148.1947118165999768, -3544.570000000000164, 2259.679250718999810 ) ) ;
#21509 = CIRCLE ( 'NONE', #11028, 5.715000000000999947 ) ;
#21510 = VECTOR ( 'NONE', #3696, 1000.000000000000000 ) ;
#21511 = LINE ( 'NONE', #1702, #22892 ) ;
#21512 = FACE_OUTER_BOUND ( 'NONE', #14316, .T. ) ;
#21513 = VECTOR ( 'NONE', #11613, 1000.000000000000114 ) ;
#21514 = ORIENTED_EDGE ( 'NONE', *, *, #4955, .F. ) ;
#21515 = CARTESIAN_POINT ( 'NONE',  ( 134.6199999999999761, -3659.504999999999654, 2244.978999999999814 ) ) ;
#21516 = DIRECTION ( 'NONE',  ( 1.000000000000000000, 0.000000000000000000, 0.000000000000000000 ) ) ;
#21517 = CARTESIAN_POINT ( 'NONE',  ( 9.855200000000998273, -3579.494999999999891, 2256.063560000000052 ) ) ;
#21518 = DIRECTION ( 'NONE',  ( 0.000000000000000000, 0.000000000000000000, -1.000000000000000000 ) ) ;
#21519 = DIRECTION ( 'NONE',  ( 0.000000000000000000, 0.000000000000000000, 1.000000000000000000 ) ) ;
#21520 = DIRECTION ( 'NONE',  ( -1.000000000000000000, 0.000000000000000000, 0.000000000000000000 ) ) ;
#21521 = ORIENTED_EDGE ( 'NONE', *, *, #14596, .F. ) ;
#21522 = CARTESIAN_POINT ( 'NONE',  ( 38.10000000000000142, -3644.899999999999636, 2239.771999999999935 ) ) ;
#21523 = AXIS2_PLACEMENT_3D ( 'NONE', #10706, #18083, #16438 ) ;
#21524 = CARTESIAN_POINT ( 'NONE',  ( -12.31900000000000084, -3662.832400000000234, 2247.392000000000280 ) ) ;
#21525 = AXIS2_PLACEMENT_3D ( 'NONE', #12320, #14661, #11248 ) ;
#21526 = CARTESIAN_POINT ( 'NONE',  ( 12.69999999999999929, -3639.502500000000055, 2264.841800000000148 ) ) ;
#21527 = APPLIED_PERSON_AND_ORGANIZATION_ASSIGNMENT ( #11036, #7759, ( #1759 ) ) ;
#21528 = DIRECTION ( 'NONE',  ( 0.000000000000000000, -1.000000000000000000, 0.000000000000000000 ) ) ;
#21529 = CIRCLE ( 'NONE', #1676, 3.606799999999993567 ) ;
#21530 = CARTESIAN_POINT ( 'NONE',  ( 142.2650958631953699, -3544.173420540363168, 2255.711176449677623 ) ) ;
#21531 = DIRECTION ( 'NONE',  ( -1.417468298637000021E-14, -1.000000000000000000, -1.319534125277000180E-12 ) ) ;
#21532 = ORIENTED_EDGE ( 'NONE', *, *, #19760, .F. ) ;
#21533 = CARTESIAN_POINT ( 'NONE',  ( 7.263164726804554050, -3577.728755824955442, 2244.777032313797463 ) ) ;
#21534 = ORIENTED_EDGE ( 'NONE', *, *, #11713, .F. ) ;
#21535 = EDGE_CURVE ( 'NONE', #22532, #4791, #1476, .T. ) ;
#21536 = CARTESIAN_POINT ( 'NONE',  ( -8.890000000036000216, -3580.206200000000081, 2245.060313203000078 ) ) ;
#21537 = EDGE_CURVE ( 'NONE', #10186, #22006, #945, .T. ) ;
#21538 = CARTESIAN_POINT ( 'NONE',  ( 10.11273377225878889, -3543.933445092538022, 2255.655515828512762 ) ) ;
#21539 = APPROVAL_DATE_TIME ( #7022, #6767 ) ;
#21540 = EDGE_CURVE ( 'NONE', #7425, #5186, #3206, .T. ) ;
#21541 = CARTESIAN_POINT ( 'NONE',  ( 0.7620000000000000107, -3543.299999999999727, 2275.763800000000174 ) ) ;
#21542 = CARTESIAN_POINT ( 'NONE',  ( 11.88149704131999940, -3656.775771668999823, 2257.621751704000417 ) ) ;
#21543 = DIRECTION ( 'NONE',  ( 0.000000000000000000, 1.000000000000000000, 0.000000000000000000 ) ) ;
#21544 = VECTOR ( 'NONE', #16890, 1000.000000000000000 ) ;
#21545 = DIRECTION ( 'NONE',  ( 0.000000000000000000, 0.000000000000000000, -1.000000000000000000 ) ) ;
#21546 = AXIS2_PLACEMENT_3D ( 'NONE', #16274, #7373, #14525 ) ;
#21547 = AXIS2_PLACEMENT_3D ( 'NONE', #3524, #1781, #23 ) ;
#21548 = DIRECTION ( 'NONE',  ( 0.7249994335945980639, 0.000000000000000000, 0.6887494619144990393 ) ) ;
#21549 = ORIENTED_EDGE ( 'NONE', *, *, #20262, .T. ) ;
#21550 = CARTESIAN_POINT ( 'NONE',  ( 35.56000000000000227, -3544.570000000000164, 2247.392000000000280 ) ) ;
#21551 = CARTESIAN_POINT ( 'NONE',  ( 9.855201422231997910, -3639.502499925999928, 2279.447341858000073 ) ) ;
#21552 = ORIENTED_EDGE ( 'NONE', *, *, #21689, .T. ) ;
#21553 = CARTESIAN_POINT ( 'NONE',  ( 151.1299999999999955, -3544.570000000000164, 2259.329999999999927 ) ) ;
#21554 = ORIENTED_EDGE ( 'NONE', *, *, #15830, .T. ) ;
#21555 = DIRECTION ( 'NONE',  ( -2.330758767204999802E-14, -1.000000000000000000, -1.206582004152999850E-12 ) ) ;
#21556 = DIRECTION ( 'NONE',  ( 0.000000000000000000, 0.000000000000000000, 1.000000000000000000 ) ) ;
#21557 = AXIS2_PLACEMENT_3D ( 'NONE', #19589, #14977, #20 ) ;
#21558 = AXIS2_PLACEMENT_3D ( 'NONE', #2321, #560, #7709 ) ;
#21559 = ORIENTED_EDGE ( 'NONE', *, *, #1366, .T. ) ;
#21560 = CIRCLE ( 'NONE', #8088, 1.269999999999882334 ) ;
#21561 = EDGE_CURVE ( 'NONE', #21114, #21667, #5467, .T. ) ;
#21562 = CARTESIAN_POINT ( 'NONE',  ( 0.7620000000000000107, -3695.699999999999818, 2239.771999999999935 ) ) ;
#21563 = ORIENTED_EDGE ( 'NONE', *, *, #14596, .T. ) ;
#21564 = CYLINDRICAL_SURFACE ( 'NONE', #10374, 0.3809999999999993947 ) ;
#21565 = AXIS2_PLACEMENT_3D ( 'NONE', #6877, #14020, #3576 ) ;
#21566 = ADVANCED_FACE ( 'NONE', ( #3589 ), #19645, .F. ) ;
#21567 = PERSON_AND_ORGANIZATION ( #5446, #1895 ) ;
#21568 = EDGE_CURVE ( 'NONE', #16359, #10014, #20787, .T. ) ;
#21569 = VECTOR ( 'NONE', #13717, 1000.000000000000000 ) ;
#21570 = DIRECTION ( 'NONE',  ( 0.000000000000000000, 0.000000000000000000, 1.000000000000000000 ) ) ;
#21571 = VECTOR ( 'NONE', #6615, 1000.000000000000000 ) ;
#21572 = CARTESIAN_POINT ( 'NONE',  ( 95.25000000000000000, -3568.700000000000273, 2244.547199999999975 ) ) ;
#21573 = DIRECTION ( 'NONE',  ( 6.119339505807659940E-14, -1.000000000000000000, 0.000000000000000000 ) ) ;
#21574 = FACE_OUTER_BOUND ( 'NONE', #9807, .T. ) ;
#21575 = CIRCLE ( 'NONE', #5860, 3.606800000000021100 ) ;
#21576 = CARTESIAN_POINT ( 'NONE',  ( 141.7174201517051131, -3577.487138885433524, 2249.884650219001742 ) ) ;
#21577 = VERTEX_POINT ( 'NONE', #16131 ) ;
#21578 = CIRCLE ( 'NONE', #22675, 2.844800000000091700 ) ;
#21579 = CARTESIAN_POINT ( 'NONE',  ( 134.9664275409213587, -3576.291810119500042, 2246.166055327845697 ) ) ;
#21580 = CARTESIAN_POINT ( 'NONE',  ( 14.50488223892000050, -3577.289998514000217, 2257.739442581999810 ) ) ;
#21581 = ORIENTED_EDGE ( 'NONE', *, *, #1656, .F. ) ;
#21582 = ADVANCED_FACE ( 'NONE', ( #17645 ), #6660, .F. ) ;
#21583 = CARTESIAN_POINT ( 'NONE',  ( 15.54479999999999862, -3599.392331916999865, 2279.447335734999797 ) ) ;
#21584 = DIRECTION ( 'NONE',  ( 0.000000000000000000, 0.000000000000000000, 1.000000000000000000 ) ) ;
#21585 = AXIS2_PLACEMENT_3D ( 'NONE', #186, #4731, #4609 ) ;
#21586 = ORIENTED_EDGE ( 'NONE', *, *, #9071, .F. ) ;
#21587 = DIRECTION ( 'NONE',  ( -0.7249994335945011414, 6.625572310375012166E-14, 0.6887494619146010688 ) ) ;
#21588 = CARTESIAN_POINT ( 'NONE',  ( 15.03168679716000078, -3655.466399999999794, 2242.820000000000164 ) ) ;
#21589 = VERTEX_POINT ( 'NONE', #10270 ) ;
#21590 = CARTESIAN_POINT ( 'NONE',  ( 20.32000000000000028, -3543.299999999999727, 2289.213099999999940 ) ) ;
#21591 = CARTESIAN_POINT ( 'NONE',  ( 12.59469521408999881, -3642.347298742000021, 2279.817638609000369 ) ) ;
#21592 =( NAMED_UNIT ( * ) SI_UNIT ( $, .STERADIAN. ) SOLID_ANGLE_UNIT ( ) );
#21593 = DIRECTION ( 'NONE',  ( -1.000000000000000000, 0.000000000000000000, 0.000000000000000000 ) ) ;
#21594 = CARTESIAN_POINT ( 'NONE',  ( 12.69999999999999929, -3579.494999999999891, 2239.009999999999764 ) ) ;
#21595 = PERSON_AND_ORGANIZATION ( #5446, #1895 ) ;
#21596 = AXIS2_PLACEMENT_3D ( 'NONE', #11867, #15965, #3422 ) ;
#21597 = DIRECTION ( 'NONE',  ( 0.000000000000000000, 0.000000000000000000, 1.000000000000000000 ) ) ;
#21598 = CARTESIAN_POINT ( 'NONE',  ( 9.832632294452492872, -3695.617810904429916, 2254.953892138222272 ) ) ;
#21599 = EDGE_LOOP ( 'NONE', ( #21216, #14368, #3575, #1113 ) ) ;
#21600 = CARTESIAN_POINT ( 'NONE',  ( 18.28253570787369142, -3580.718563225802882, 2245.237727082001129 ) ) ;
#21601 = VECTOR ( 'NONE', #1997, 1000.000000000000114 ) ;
#21602 = AXIS2_PLACEMENT_3D ( 'NONE', #18535, #832, #19003 ) ;
#21603 = EDGE_CURVE ( 'NONE', #13127, #12999, #7336, .T. ) ;
#21604 = FACE_OUTER_BOUND ( 'NONE', #7138, .T. ) ;
#21605 = ADVANCED_FACE ( 'NONE', ( #1365, #8528 ), #7010, .T. ) ;
#21606 = TOROIDAL_SURFACE ( 'NONE', #16358, 3.606799999999999784, 0.7620000000000000107 ) ;
#21607 = ORIENTED_EDGE ( 'NONE', *, *, #5081, .F. ) ;
#21608 = CARTESIAN_POINT ( 'NONE',  ( 138.3834544057343976, -3662.027211347764023, 2249.520849656408245 ) ) ;
#21609 = ORIENTED_EDGE ( 'NONE', *, *, #13874, .F. ) ;
#21610 = EDGE_CURVE ( 'NONE', #14398, #12135, #20424, .T. ) ;
#21611 = ORIENTED_EDGE ( 'NONE', *, *, #4263, .F. ) ;
#21612 = DIRECTION ( 'NONE',  ( 2.324635735433000053E-14, 0.000000000000000000, 1.000000000000000000 ) ) ;
#21613 = ORIENTED_EDGE ( 'NONE', *, *, #20842, .T. ) ;
#21614 = ORIENTED_EDGE ( 'NONE', *, *, #8354, .F. ) ;
#21615 = DIRECTION ( 'NONE',  ( 0.000000000000000000, 0.000000000000000000, -1.000000000000000000 ) ) ;
#21616 = COORDINATED_UNIVERSAL_TIME_OFFSET ( 0, 0, .AHEAD. ) ;
#21617 = CARTESIAN_POINT ( 'NONE',  ( 3.810000000000000053, -3544.061999999999898, 2253.487999999999829 ) ) ;
#21618 = EDGE_CURVE ( 'NONE', #7858, #204, #15937, .T. ) ;
#21619 = ORIENTED_EDGE ( 'NONE', *, *, #5406, .F. ) ;
#21620 = DIRECTION ( 'NONE',  ( -0.6887494619136477203, 0.000000000000000000, 0.7249994335954068614 ) ) ;
#21621 = ADVANCED_FACE ( 'NONE', ( #17767 ), #19304, .T. ) ;
#21622 = DIRECTION ( 'NONE',  ( 0.000000000000000000, 0.000000000000000000, 1.000000000000000000 ) ) ;
#21623 = CARTESIAN_POINT ( 'NONE',  ( -12.31900000000000084, -3658.793800000000374, 2249.723686796999573 ) ) ;
#21624 = DIRECTION ( 'NONE',  ( 0.000000000000000000, 0.000000000000000000, -1.000000000000000000 ) ) ;
#21625 = APPROVAL_DATE_TIME ( #14481, #16798 ) ;
#21626 = ORIENTED_EDGE ( 'NONE', *, *, #7774, .T. ) ;
#21627 = CARTESIAN_POINT ( 'NONE',  ( 131.9075161311309046, -3543.615630485107431, 2260.168083407881113 ) ) ;
#21628 = VERTEX_POINT ( 'NONE', #20223 ) ;
#21629 = LINE ( 'NONE', #9321, #7207 ) ;
#21630 = EDGE_CURVE ( 'NONE', #6446, #20602, #19680, .T. ) ;
#21631 = CARTESIAN_POINT ( 'NONE',  ( 137.3683132029000262, -3660.851200000000063, 2242.820000000000164 ) ) ;
#21632 = VERTEX_POINT ( 'NONE', #19774 ) ;
#21633 = CARTESIAN_POINT ( 'NONE',  ( 151.1299999999999955, -3544.570000000000164, 2240.279999999999745 ) ) ;
#21634 = LINE ( 'NONE', #1708, #22975 ) ;
#21635 = DIRECTION ( 'NONE',  ( 0.000000000000000000, 1.000000000000000000, 0.000000000000000000 ) ) ;
#21636 = CARTESIAN_POINT ( 'NONE',  ( 142.5447999999989861, -3659.504999999999654, 2272.030000000000200 ) ) ;
#21637 = CYLINDRICAL_SURFACE ( 'NONE', #961, 2.844799999999009010 ) ;
#21638 = ORIENTED_EDGE ( 'NONE', *, *, #3562, .T. ) ;
#21639 = CARTESIAN_POINT ( 'NONE',  ( 15.54479972192533488, -3659.504999998566745, 2257.962943247991007 ) ) ;
#21640 = CARTESIAN_POINT ( 'NONE',  ( 35.25520000000000209, -3594.099999999999909, 2259.837999999999738 ) ) ;
#21641 = DIRECTION ( 'NONE',  ( -1.000000000000000000, 0.000000000000000000, 0.000000000000000000 ) ) ;
#21642 = EDGE_CURVE ( 'NONE', #20964, #6627, #10318, .T. ) ;
#21643 = AXIS2_PLACEMENT_3D ( 'NONE', #19139, #3076, #1553 ) ;
#21644 = DIRECTION ( 'NONE',  ( 0.000000000000000000, 0.000000000000000000, -1.000000000000000000 ) ) ;
#21645 = DIRECTION ( 'NONE',  ( 1.000000000000000000, 0.000000000000000000, 0.000000000000000000 ) ) ;
#21646 = CARTESIAN_POINT ( 'NONE',  ( 136.9169929778280164, -3695.514947979135286, 2255.165585416540125 ) ) ;
#21647 = ORIENTED_EDGE ( 'NONE', *, *, #9302, .T. ) ;
#21648 = CARTESIAN_POINT ( 'NONE',  ( 25.39999999999999858, -3578.860000000000127, 2250.236800000000130 ) ) ;
#21649 = ORIENTED_EDGE ( 'NONE', *, *, #4293, .F. ) ;
#21650 = APPROVAL_STATUS ( 'not_yet_approved' ) ;
#21651 = CARTESIAN_POINT ( 'NONE',  ( 47.19319999999999737, -3568.700000000000273, 2259.837999999999738 ) ) ;
#21652 = CARTESIAN_POINT ( 'NONE',  ( 15.03168679714000078, -3638.156300000000101, 2296.210799999999836 ) ) ;
#21653 = CALENDAR_DATE ( 2026, 26, 10 ) ;
#21654 = CARTESIAN_POINT ( 'NONE',  ( -6.349999999999999645, -3573.399000000000342, 2247.392000000000280 ) ) ;
#21655 = DIRECTION ( 'NONE',  ( 0.000000000000000000, 0.000000000000000000, -1.000000000000000000 ) ) ;
#21656 = DIRECTION ( 'NONE',  ( 0.000000000000000000, 0.000000000000000000, -1.000000000000000000 ) ) ;
#21657 = CARTESIAN_POINT ( 'NONE',  ( 92.50679999999999836, -3594.099999999999909, 2239.771999999999935 ) ) ;
#21658 = APPLIED_PERSON_AND_ORGANIZATION_ASSIGNMENT ( #4540, #1138, ( #2620 ) ) ;
#21659 = ORIENTED_EDGE ( 'NONE', *, *, #7864, .T. ) ;
#21660 = CARTESIAN_POINT ( 'NONE',  ( 132.3005794017000198, -3544.570000000000164, 2260.390449568000349 ) ) ;
#21661 = ORIENTED_EDGE ( 'NONE', *, *, #10950, .F. ) ;
#21662 = VECTOR ( 'NONE', #3007, 1000.000000000000000 ) ;
#21663 = DIRECTION ( 'NONE',  ( -1.000000000000000000, 0.000000000000000000, 0.000000000000000000 ) ) ;
#21664 = DIRECTION ( 'NONE',  ( 0.000000000000000000, 0.000000000000000000, -1.000000000000000000 ) ) ;
#21665 = VERTEX_POINT ( 'NONE', #12729 ) ;
#21666 = DIRECTION ( 'NONE',  ( 0.000000000000000000, 0.000000000000000000, -1.000000000000000000 ) ) ;
#21667 = VERTEX_POINT ( 'NONE', #16470 ) ;
#21668 = CARTESIAN_POINT ( 'NONE',  ( 142.3627523022312857, -3695.258941566818521, 2255.466570801501348 ) ) ;
#21669 = FACE_OUTER_BOUND ( 'NONE', #15514, .T. ) ;
#21670 = ORIENTED_EDGE ( 'NONE', *, *, #10737, .T. ) ;
#21671 = CARTESIAN_POINT ( 'NONE',  ( 137.8189483952010903, -3581.629460150263640, 2248.048772148962144 ) ) ;
#21672 = VERTEX_POINT ( 'NONE', #9336 ) ;
#21673 = AXIS2_PLACEMENT_3D ( 'NONE', #23036, #12383, #3590 ) ;
#21674 = CARTESIAN_POINT ( 'NONE',  ( 0.000000000000000000, -3544.570000000000164, 2240.279999999999745 ) ) ;
#21675 = DATE_TIME_ROLE ( 'creation_date' ) ;
#21676 = DIRECTION ( 'NONE',  ( 0.000000000000000000, 0.000000000000000000, -1.000000000000000000 ) ) ;
#21677 = CARTESIAN_POINT ( 'NONE',  ( 146.1769999999999925, -3659.504999999999654, 2239.009999999999764 ) ) ;
#21678 = CARTESIAN_POINT ( 'NONE',  ( 3.044261469311703827, -3543.299999999971988, 2275.317430734553909 ) ) ;
#21679 = APPLIED_DATE_AND_TIME_ASSIGNMENT ( #18688, #16926, ( #10933 ) ) ;
#21680 = CYLINDRICAL_SURFACE ( 'NONE', #22187, 5.460999999999938126 ) ;
#21681 = CARTESIAN_POINT ( 'NONE',  ( 139.0560147878972828, -3576.723841947683468, 2249.270788651956991 ) ) ;
#21682 = ORIENTED_EDGE ( 'NONE', *, *, #9652, .F. ) ;
#21683 = CARTESIAN_POINT ( 'NONE',  ( 134.6682978865242148, -3576.785158905799108, 2245.445731933577008 ) ) ;
#21684 = AXIS2_PLACEMENT_3D ( 'NONE', #8859, #16003, #12259 ) ;
#21685 = EDGE_CURVE ( 'NONE', #11125, #3802, #7567, .T. ) ;
#21686 = VERTEX_POINT ( 'NONE', #3701 ) ;
#21687 = DIRECTION ( 'NONE',  ( 0.000000000000000000, 0.000000000000000000, -1.000000000000000000 ) ) ;
#21688 = ORIENTED_EDGE ( 'NONE', *, *, #18117, .F. ) ;
#21689 = EDGE_CURVE ( 'NONE', #18533, #796, #14379, .T. ) ;
#21690 = CARTESIAN_POINT ( 'NONE',  ( 11.61844525849999954, -3582.131125288000021, 2257.644379465999918 ) ) ;
#21691 = AXIS2_PLACEMENT_3D ( 'NONE', #6142, #18434, #20202 ) ;
#21692 = CARTESIAN_POINT ( 'NONE',  ( 111.4552000000009997, -3644.899999999999636, 2259.837999999999738 ) ) ;
#21693 = EDGE_CURVE ( 'NONE', #2966, #3298, #8082, .T. ) ;
#21694 = ORIENTED_EDGE ( 'NONE', *, *, #18022, .F. ) ;
#21695 = CARTESIAN_POINT ( 'NONE',  ( 151.4000000000000057, -3544.061999999999898, 2279.827800000000025 ) ) ;
#21696 = CARTESIAN_POINT ( 'NONE',  ( 139.6999999999999886, -3659.504999999999654, 2239.009999999999764 ) ) ;
#21697 = ORIENTED_EDGE ( 'NONE', *, *, #18113, .T. ) ;
#21698 = CARTESIAN_POINT ( 'NONE',  ( 88.90000000000000568, -3594.099999999999909, 2261.869999999999891 ) ) ;
#21699 = CARTESIAN_POINT ( 'NONE',  ( 60.21459350834000190, -3544.061999999999898, 2280.170699136999701 ) ) ;
#21700 = CARTESIAN_POINT ( 'NONE',  ( 144.7800000000000011, -3579.494999999999891, 2239.009999999999764 ) ) ;
#21701 = CARTESIAN_POINT ( 'NONE',  ( 139.6999999999986528, -3662.197400000179641, 2239.167815367330604 ) ) ;
#21702 = PERSON_AND_ORGANIZATION_ROLE ( 'design_supplier' ) ;
#21703 = EDGE_LOOP ( 'NONE', ( #14774, #9680, #22135, #21715 ) ) ;
#21704 = AXIS2_PLACEMENT_3D ( 'NONE', #3626, #12541, #17689 ) ;
#21705 = CARTESIAN_POINT ( 'NONE',  ( 60.65520000000000067, -3594.099999999999909, 2239.771999999999935 ) ) ;
#21706 = CARTESIAN_POINT ( 'NONE',  ( 98.75520000000000209, -3568.700000000000273, 2239.771999999999935 ) ) ;
#21707 = ORIENTED_EDGE ( 'NONE', *, *, #3504, .F. ) ;
#21708 = LOCAL_TIME ( 17, 37, 43.00000000000000000, #21929 ) ;
#21709 = DIRECTION ( 'NONE',  ( -1.000000000000000000, 0.000000000000000000, 0.000000000000000000 ) ) ;
#21710 = EDGE_CURVE ( 'NONE', #9431, #9937, #19710, .T. ) ;
#21711 = AXIS2_PLACEMENT_3D ( 'NONE', #4569, #13365, #3040 ) ;
#21712 = CARTESIAN_POINT ( 'NONE',  ( 137.8779939444977458, -3657.320203822652729, 2246.982792015143787 ) ) ;
#21713 = ORIENTED_EDGE ( 'NONE', *, *, #47, .F. ) ;
#21714 = CARTESIAN_POINT ( 'NONE',  ( 137.2246884197096222, -3660.907179621593968, 2250.131455798929437 ) ) ;
#21715 = ORIENTED_EDGE ( 'NONE', *, *, #22968, .F. ) ;
#21716 = VERTEX_POINT ( 'NONE', #18231 ) ;
#21717 = VECTOR ( 'NONE', #6066, 1000.000000000000000 ) ;
#21718 = EDGE_CURVE ( 'NONE', #18263, #4281, #7458, .T. ) ;
#21719 = DIRECTION ( 'NONE',  ( 0.000000000000000000, -1.000000000000000000, 0.000000000000000000 ) ) ;
#21720 = ORIENTED_EDGE ( 'NONE', *, *, #14853, .F. ) ;
#21721 = ORIENTED_EDGE ( 'NONE', *, *, #3904, .F. ) ;
#21722 = LOCAL_TIME ( 17, 37, 43.00000000000000000, #6550 ) ;
#21723 = CARTESIAN_POINT ( 'NONE',  ( 15.54479999999932716, -3659.053785370524565, 2256.063560000000962 ) ) ;
#21724 = LINE ( 'NONE', #16336, #12907 ) ;
#21725 = LOCAL_TIME ( 17, 37, 43.00000000000000000, #17680 ) ;
#21726 = EDGE_CURVE ( 'NONE', #3332, #22386, #9446, .T. ) ;
#21727 = EDGE_LOOP ( 'NONE', ( #10036, #23056, #387, #562 ) ) ;
#21728 = ADVANCED_FACE ( 'NONE', ( #11309 ), #18460, .F. ) ;
#21729 = CARTESIAN_POINT ( 'NONE',  ( -6.349999999999999645, -3660.140000000000327, 2247.392000000000280 ) ) ;
#21730 = CARTESIAN_POINT ( 'NONE',  ( 7.289238816486445671, -3581.334923857885769, 2245.989158447137015 ) ) ;
#21731 = CARTESIAN_POINT ( 'NONE',  ( 53.64479999999999649, -3619.500000000000000, 2261.869999999999891 ) ) ;
#21732 = APPROVAL_ROLE ( '' ) ;
#21733 = CARTESIAN_POINT ( 'NONE',  ( 88.90000000000000568, -3644.899999999999636, 2261.869999999999891 ) ) ;
#21734 = ORIENTED_EDGE ( 'NONE', *, *, #22968, .T. ) ;
#21735 = CYLINDRICAL_SURFACE ( 'NONE', #5334, 5.460999999999938126 ) ;
#21736 = CARTESIAN_POINT ( 'NONE',  ( 35.56000000000000227, -3670.300000000000182, 2247.392000000000280 ) ) ;
#21737 = LOCAL_TIME ( 17, 37, 43.00000000000000000, #18839 ) ;
#21738 = LOCAL_TIME ( 17, 37, 43.00000000000000000, #759 ) ;
#21739 = DIRECTION ( 'NONE',  ( -1.000000000000000000, 0.000000000000000000, 0.000000000000000000 ) ) ;
#21740 = ORIENTED_EDGE ( 'NONE', *, *, #4610, .T. ) ;
#21741 = EDGE_CURVE ( 'NONE', #14294, #10396, #14612, .T. ) ;
#21742 = CARTESIAN_POINT ( 'NONE',  ( 129.8447999999989975, -3568.700000000000273, 2259.837999999999738 ) ) ;
#21743 = DIRECTION ( 'NONE',  ( 0.000000000000000000, 0.000000000000000000, 1.000000000000000000 ) ) ;
#21744 = DIRECTION ( 'NONE',  ( 1.000000000000000000, 0.000000000000000000, 0.000000000000000000 ) ) ;
#21745 = DIRECTION ( 'NONE',  ( 0.000000000000000000, 0.000000000000000000, -1.000000000000000000 ) ) ;
#21746 = PRODUCT_DEFINITION_SHAPE ( 'NONE', 'NONE',  #23174 ) ;
#21747 = AXIS2_PLACEMENT_3D ( 'NONE', #7537, #16102, #14696 ) ;
#21748 = CARTESIAN_POINT ( 'NONE',  ( 147.6473055386096007, -3543.381058770634354, 2259.780196767977031 ) ) ;
#21749 = ORIENTED_EDGE ( 'NONE', *, *, #762, .T. ) ;
#21750 = CARTESIAN_POINT ( 'NONE',  ( 147.5486189909101995, -3695.492037868064472, 2260.027647172040361 ) ) ;
#21751 = CYLINDRICAL_SURFACE ( 'NONE', #4356, 6.349999999999855760 ) ;
#21752 = EDGE_CURVE ( 'NONE', #15774, #14725, #9924, .T. ) ;
#21753 = DIRECTION ( 'NONE',  ( -2.334777064352623371E-14, -1.000000000000000000, 0.000000000000000000 ) ) ;
#21754 = DIRECTION ( 'NONE',  ( 0.000000000000000000, 0.000000000000000000, 1.000000000000000000 ) ) ;
#21755 = DIRECTION ( 'NONE',  ( 1.097617497454356000E-13, 0.000000000000000000, 1.000000000000000000 ) ) ;
#21756 = LOCAL_TIME ( 17, 37, 43.00000000000000000, #17735 ) ;
#21757 =( BOUNDED_CURVE ( )  B_SPLINE_CURVE ( 3, ( #8168, #17174, #7936, #15429 ),
 .UNSPECIFIED., .F., .T. ) 
 B_SPLINE_CURVE_WITH_KNOTS ( ( 4, 4 ),
 ( 3.686081134657729747E-14, 1.570796326492095440 ),
 .UNSPECIFIED. ) 
 CURVE ( )  GEOMETRIC_REPRESENTATION_ITEM ( )  RATIONAL_B_SPLINE_CURVE ( ( 1.000000000000000000, 0.8047378541957446174, 0.8047378541957446174, 1.000000000000000000 ) ) 
 REPRESENTATION_ITEM ( '' )  );
#21758 = CARTESIAN_POINT ( 'NONE',  ( 12.69999999999999929, -3583.940000000000055, 2262.355140000000119 ) ) ;
#21759 = ORIENTED_EDGE ( 'NONE', *, *, #4547, .T. ) ;
#21760 = PERSON_AND_ORGANIZATION ( #5446, #1895 ) ;
#21761 = CARTESIAN_POINT ( 'NONE',  ( -12.31900000000000084, -3661.486200000121244, 2249.723686796789480 ) ) ;
#21762 = ADVANCED_FACE ( 'NONE', ( #9555 ), #21751, .T. ) ;
#21763 = FACE_OUTER_BOUND ( 'NONE', #895, .T. ) ;
#21764 = CIRCLE ( 'NONE', #9766, 0.7619999999999987894 ) ;
#21765 = DATE_AND_TIME ( #14625, #8270 ) ;
#21766 = AXIS2_PLACEMENT_3D ( 'NONE', #1780, #3752, #8924 ) ;
#21767 = DIRECTION ( 'NONE',  ( 1.000000000000000000, 0.000000000000000000, 0.000000000000000000 ) ) ;
#21768 = DIRECTION ( 'NONE',  ( 0.000000000000000000, -1.000000000000000000, 0.000000000000000000 ) ) ;
#21769 = EDGE_CURVE ( 'NONE', #9361, #796, #4705, .T. ) ;
#21770 = CARTESIAN_POINT ( 'NONE',  ( 76.20000000000000284, -3568.700000000000273, 2239.009999999999764 ) ) ;
#21771 =( REPRESENTATION_RELATIONSHIP ('NONE','NONE', #20448, #15665 ) REPRESENTATION_RELATIONSHIP_WITH_TRANSFORMATION ( #5607 )SHAPE_REPRESENTATION_RELATIONSHIP( ) );
#21772 = EDGE_CURVE ( 'NONE', #2000, #2498, #12589, .T. ) ;
#21773 = ORIENTED_EDGE ( 'NONE', *, *, #1350, .T. ) ;
#21774 = DIRECTION ( 'NONE',  ( 1.000000000000000000, 0.000000000000000000, 0.000000000000000000 ) ) ;
#21775 = EDGE_LOOP ( 'NONE', ( #4466, #16827, #12808, #22830, #1527, #7119, #1172, #6779, #14871, #5114, #21586, #640 ) ) ;
#21776 = DIRECTION ( 'NONE',  ( 0.000000000000000000, 0.000000000000000000, -1.000000000000000000 ) ) ;
#21777 = PLANE ( 'NONE',  #2839 ) ;
#21778 = ORIENTED_EDGE ( 'NONE', *, *, #20465, .F. ) ;
#21779 = DIRECTION ( 'NONE',  ( 0.000000000000000000, 0.000000000000000000, -1.000000000000000000 ) ) ;
#21780 = VECTOR ( 'NONE', #17487, 1000.000000000000114 ) ;
#21781 = AXIS2_PLACEMENT_3D ( 'NONE', #15123, #20613, #11255 ) ;
#21782 = EDGE_LOOP ( 'NONE', ( #16325, #19215, #8687, #15985 ) ) ;
#21783 = CARTESIAN_POINT ( 'NONE',  ( 142.5673055393761786, -3695.618941230270593, 2254.954196765868346 ) ) ;
#21784 = ORIENTED_EDGE ( 'NONE', *, *, #8781, .F. ) ;
#21785 = CARTESIAN_POINT ( 'NONE',  ( 137.8884899131788586, -3581.688494919837467, 2247.706546665592668 ) ) ;
#21786 = ORIENTED_EDGE ( 'NONE', *, *, #1621, .T. ) ;
#21787 = DIRECTION ( 'NONE',  ( 0.000000000000000000, 0.000000000000000000, 1.000000000000000000 ) ) ;
#21789 = AXIS2_PLACEMENT_3D ( 'NONE', #11652, #9566, #16931 ) ;
#21788 = PERSON_AND_ORGANIZATION_ROLE ( 'classification_officer' ) ;
#21790 = CYLINDRICAL_SURFACE ( 'NONE', #18691, 2.844799999999994444 ) ;
#21791 = FACE_BOUND ( 'NONE', #7919, .T. ) ;
#21792 = VECTOR ( 'NONE', #7293, 1000.000000000000000 ) ;
#21793 = VECTOR ( 'NONE', #3135, 1000.000000000000000 ) ;
#21794 = DIRECTION ( 'NONE',  ( -4.457711412217000029E-12, 1.000000000000000000, 0.000000000000000000 ) ) ;
#21795 = CARTESIAN_POINT ( 'NONE',  ( 9.864068217991999177, -3579.219970543999807, 2257.960591680000107 ) ) ;
#21796 = VECTOR ( 'NONE', #2218, 1000.000000000000114 ) ;
#21797 = CARTESIAN_POINT ( 'NONE',  ( 138.1443562676044223, -3577.112753218966191, 2249.637217027982842 ) ) ;
#21798 = ORIENTED_EDGE ( 'NONE', *, *, #18857, .T. ) ;
#21799 = CARTESIAN_POINT ( 'NONE',  ( 134.0354590894625915, -3578.735571264413466, 2244.549527799902535 ) ) ;
#21800 = ORIENTED_EDGE ( 'NONE', *, *, #1540, .T. ) ;
#21801 = CARTESIAN_POINT ( 'NONE',  ( 127.0000000000000000, -3578.860000000000127, 2247.392000000000280 ) ) ;
#21802 = ORIENTED_EDGE ( 'NONE', *, *, #19026, .F. ) ;
#21803 = CARTESIAN_POINT ( 'NONE',  ( 14.93205609083999974, -3597.723870509999870, 2279.591813517999981 ) ) ;
#21804 = DIRECTION ( 'NONE',  ( 0.000000000000000000, -1.000000000000000000, 0.000000000000000000 ) ) ;
#21805 = CIRCLE ( 'NONE', #19936, 2.844799999999009010 ) ;
#21806 = ORIENTED_EDGE ( 'NONE', *, *, #9438, .T. ) ;
#21807 = DIRECTION ( 'NONE',  ( 0.000000000000000000, 1.000000000000000000, 0.000000000000000000 ) ) ;
#21808 = DIRECTION ( 'NONE',  ( 0.000000000000000000, -1.000000000000000000, 0.000000000000000000 ) ) ;
#21809 = CIRCLE ( 'NONE', #13578, 0.7619999999999294005 ) ;
#21810 = ORIENTED_EDGE ( 'NONE', *, *, #21820, .F. ) ;
#21811 = APPROVAL ( #13624, 'UNSPECIFIED' ) ;
#21812 = AXIS2_PLACEMENT_3D ( 'NONE', #8472, #21123, #3181 ) ;
#21813 = DIRECTION ( 'NONE',  ( 0.000000000000000000, 1.000000000000000000, 0.000000000000000000 ) ) ;
#21814 = CARTESIAN_POINT ( 'NONE',  ( 9.919062418924999847, -3640.129156706999765, 2279.464122714000041 ) ) ;
#21815 = CARTESIAN_POINT ( 'NONE',  ( 141.5113688234855545, -3581.688645776049725, 2247.086479173670796 ) ) ;
#21816 = EDGE_LOOP ( 'NONE', ( #19715, #12605, #11724, #10250 ) ) ;
#21817 = DIRECTION ( 'NONE',  ( 1.000000000000000000, 1.206643234470999950E-12, 0.000000000000000000 ) ) ;
#21818 = APPROVAL_ROLE ( '' ) ;
#21819 = AXIS2_PLACEMENT_3D ( 'NONE', #19396, #12123, #3449 ) ;
#21820 = EDGE_CURVE ( 'NONE', #10484, #3518, #18563, .T. ) ;
#21821 = CARTESIAN_POINT ( 'NONE',  ( 137.3683132029000262, -3578.148799999999937, 2242.820000000000164 ) ) ;
#21822 = DIRECTION ( 'NONE',  ( 0.000000000000000000, 0.000000000000000000, -1.000000000000000000 ) ) ;
#21823 = ORIENTED_EDGE ( 'NONE', *, *, #10437, .T. ) ;
#21825 = ADVANCED_FACE ( 'NONE', ( #5599 ), #19883, .T. ) ;
#21824 = CARTESIAN_POINT ( 'NONE',  ( 1.270000000000000018, -3694.430000000000291, 2240.279999999999745 ) ) ;
#21826 = AXIS2_PLACEMENT_3D ( 'NONE', #20717, #10053, #19083 ) ;
#21827 = ADVANCED_FACE ( 'NONE', ( #16702, #17154 ), #22082, .T. ) ;
#21828 = CARTESIAN_POINT ( 'NONE',  ( 12.69999999999999929, -3659.504999999999654, 2239.391000000000076 ) ) ;
#21829 = EDGE_LOOP ( 'NONE', ( #16367, #10528, #22488, #2004 ) ) ;
#21830 = ORIENTED_EDGE ( 'NONE', *, *, #1697, .F. ) ;
#21831 = VECTOR ( 'NONE', #9313, 1000.000000000000000 ) ;
#21832 = CARTESIAN_POINT ( 'NONE',  ( 138.8454383216908070, -3662.218504070199288, 2249.334367105925594 ) ) ;
#21833 = ADVANCED_FACE ( 'NONE', ( #14952 ), #13645, .T. ) ;
#21834 = ORIENTED_EDGE ( 'NONE', *, *, #14540, .F. ) ;
#21835 = ORIENTED_EDGE ( 'NONE', *, *, #10438, .T. ) ;
#21836 = DIRECTION ( 'NONE',  ( 1.000000000000000000, 0.000000000000000000, 3.996303350731721563E-14 ) ) ;
#21837 = ORIENTED_EDGE ( 'NONE', *, *, #11102, .T. ) ;
#21838 = DIRECTION ( 'NONE',  ( 0.000000000000000000, -1.000000000000000000, 0.000000000000000000 ) ) ;
#21839 = EDGE_CURVE ( 'NONE', #14116, #13045, #14468, .T. ) ;
#21840 = CARTESIAN_POINT ( 'NONE',  ( 110.6932000000009992, -3644.899999999999636, 2260.600000000000364 ) ) ;
#21841 = CIRCLE ( 'NONE', #7258, 1.269999999999882334 ) ;
#21842 = ORIENTED_EDGE ( 'NONE', *, *, #15826, .F. ) ;
#21843 = CARTESIAN_POINT ( 'NONE',  ( -12.31899999999998663, -3662.832400000169400, 2247.392000000001190 ) ) ;
#21844 = CIRCLE ( 'NONE', #11723, 2.844800000000091700 ) ;
#21845 = CARTESIAN_POINT ( 'NONE',  ( 7.197112922637037613, -3581.033299165524113, 2245.555178679493110 ) ) ;
#21846 = CYLINDRICAL_SURFACE ( 'NONE', #3277, 0.7619999999999294005 ) ;
#21847 = PERSON_AND_ORGANIZATION_ROLE ( 'design_owner' ) ;
#21848 = VECTOR ( 'NONE', #16066, 1000.000000000000000 ) ;
#21849 = DIRECTION ( 'NONE',  ( 0.000000000000000000, 0.000000000000000000, -1.000000000000000000 ) ) ;
#21850 = EDGE_CURVE ( 'NONE', #15909, #20725, #8604, .T. ) ;
#21851 = EDGE_CURVE ( 'NONE', #18372, #4050, #2741, .T. ) ;
#21852 = CARTESIAN_POINT ( 'NONE',  ( 63.50000000000000000, -3644.899999999999636, 2259.837999999999738 ) ) ;
#21853 = ORIENTED_EDGE ( 'NONE', *, *, #13811, .T. ) ;
#21854 = DIRECTION ( 'NONE',  ( 0.000000000000000000, -1.000000000000000000, 0.000000000000000000 ) ) ;
#21855 = VERTEX_POINT ( 'NONE', #13182 ) ;
#21856 = AXIS2_PLACEMENT_3D ( 'NONE', #7475, #14518, #14746 ) ;
#21857 = CARTESIAN_POINT ( 'NONE',  ( 35.56000000000000227, -3695.699999999999818, 2243.277199999999993 ) ) ;
#21858 = DIRECTION ( 'NONE',  ( 0.000000000000000000, 0.000000000000000000, 1.000000000000000000 ) ) ;
#21859 = DIRECTION ( 'NONE',  ( 0.000000000000000000, 2.336881798971000105E-14, -1.000000000000000000 ) ) ;
#21860 = CARTESIAN_POINT ( 'NONE',  ( 25.39999999999999858, -3670.300000000000182, 2239.009999999999764 ) ) ;
#21861 = DIRECTION ( 'NONE',  ( -1.000000000000000000, 0.000000000000000000, 0.000000000000000000 ) ) ;
#21862 = ORIENTED_EDGE ( 'NONE', *, *, #5288, .T. ) ;
#21863 = CARTESIAN_POINT ( 'NONE',  ( 147.6177471794484859, -3695.586719555673881, 2259.854339697793421 ) ) ;
#21864 = EDGE_CURVE ( 'NONE', #8499, #15348, #3968, .T. ) ;
#21865 = CARTESIAN_POINT ( 'NONE',  ( 38.10000000000000142, -3644.899999999999636, 2239.009999999999764 ) ) ;
#21866 = CARTESIAN_POINT ( 'NONE',  ( 136.9873132028999976, -3661.071170452999922, 2239.009999999999764 ) ) ;
#21867 = CARTESIAN_POINT ( 'NONE',  ( 25.39999999999999858, -3568.700000000000273, 2239.771999999999935 ) ) ;
#21868 = CARTESIAN_POINT ( 'NONE',  ( 142.5673427038165642, -3543.381058771931293, 2254.954211610746825 ) ) ;
#21869 = CARTESIAN_POINT ( 'NONE',  ( 12.69999999999999929, -3579.494999999999891, 2245.359999999999673 ) ) ;
#21870 = DIRECTION ( 'NONE',  ( -1.000000000000000000, 0.000000000000000000, 0.000000000000000000 ) ) ;
#21871 = EDGE_LOOP ( 'NONE', ( #17384, #17146, #6270, #3788, #18783, #1327, #3970, #18986, #16628, #11034, #18544 ) ) ;
#21872 = SHAPE_DEFINITION_REPRESENTATION ( #17212, #536 ) ;
#21873 = VECTOR ( 'NONE', #14378, 1000.000000000000000 ) ;
#21874 = CARTESIAN_POINT ( 'NONE',  ( 145.3974439044723113, -3659.043045737660577, 2244.764295548285190 ) ) ;
#21875 = DIRECTION ( 'NONE',  ( 0.000000000000000000, -1.000000000000000000, 0.000000000000000000 ) ) ;
#21876 = CARTESIAN_POINT ( 'NONE',  ( 117.1447999999989946, -3594.099999999999909, 2259.837999999999738 ) ) ;
#21877 = CARTESIAN_POINT ( 'NONE',  ( 34.49320000000000164, -3594.099999999999909, 2260.600000000000364 ) ) ;
#21878 = EDGE_CURVE ( 'NONE', #18145, #20995, #13706, .T. ) ;
#21879 = ADVANCED_FACE ( 'NONE', ( #9775 ), #8150, .F. ) ;
#21880 = ADVANCED_FACE ( 'NONE', ( #4502 ), #15179, .T. ) ;
#21881 = DIRECTION ( 'NONE',  ( 0.000000000000000000, 0.000000000000000000, 1.000000000000000000 ) ) ;
#21882 = ORIENTED_EDGE ( 'NONE', *, *, #22247, .T. ) ;
#21883 = AXIS2_PLACEMENT_3D ( 'NONE', #17821, #15953, #5291 ) ;
#21884 = CARTESIAN_POINT ( 'NONE',  ( 151.4000000000000057, -3544.570000000000164, 2260.570967364599255 ) ) ;
#21885 = AXIS2_PLACEMENT_3D ( 'NONE', #18675, #529, #22300 ) ;
#21886 = DIRECTION ( 'NONE',  ( 0.000000000000000000, 0.000000000000000000, 1.000000000000000000 ) ) ;
#21887 = AXIS2_PLACEMENT_3D ( 'NONE', #6023, #14925, #9747 ) ;
#21888 = ORIENTED_EDGE ( 'NONE', *, *, #17116, .T. ) ;
#21889 = EDGE_CURVE ( 'NONE', #11527, #8900, #19037, .T. ) ;
#21890 = CARTESIAN_POINT ( 'NONE',  ( 15.54479999999999862, -3599.497499999999945, 2263.571799999999712 ) ) ;
#21891 = DIRECTION ( 'NONE',  ( 0.000000000000000000, 1.000000000000000000, 0.000000000000000000 ) ) ;
#21892 = ORIENTED_EDGE ( 'NONE', *, *, #10960, .T. ) ;
#21893 = DIRECTION ( 'NONE',  ( -1.000000000000000000, 2.330758767201999921E-14, 2.343004830739999973E-14 ) ) ;
#21894 = CARTESIAN_POINT ( 'NONE',  ( -5.588000000000000078, -3544.061999999999898, 2229.612000000000080 ) ) ;
#21895 = EDGE_CURVE ( 'NONE', #279, #5355, #18916, .T. ) ;
#21896 = ORIENTED_EDGE ( 'NONE', *, *, #21138, .F. ) ;
#21897 = EDGE_CURVE ( 'NONE', #7027, #19565, #16689, .T. ) ;
#21898 = CARTESIAN_POINT ( 'NONE',  ( 57.14999999999999858, -3694.430000000000291, 2247.392000000000280 ) ) ;
#21899 = CIRCLE ( 'NONE', #12550, 3.606799999999993567 ) ;
#21900 = ORIENTED_EDGE ( 'NONE', *, *, #12865, .T. ) ;
#21901 = CARTESIAN_POINT ( 'NONE',  ( 145.1247579277662112, -3581.293143190419869, 2245.917988638741008 ) ) ;
#21902 = CIRCLE ( 'NONE', #217, 5.080000000000000959 ) ;
#21903 = COORDINATED_UNIVERSAL_TIME_OFFSET ( 0, 0, .AHEAD. ) ;
#21904 = VECTOR ( 'NONE', #15696, 1000.000000000000000 ) ;
#21905 = AXIS2_PLACEMENT_3D ( 'NONE', #7511, #11027, #5542 ) ;
#21906 = LINE ( 'NONE', #18616, #6366 ) ;
#21907 = CARTESIAN_POINT ( 'NONE',  ( 17.58063922156827630, -3662.478349466719010, 2245.771667880976565 ) ) ;
#21908 = CARTESIAN_POINT ( 'NONE',  ( 12.69999999999999929, -3596.322499999999764, 2290.241799999999785 ) ) ;
#21909 = LINE ( 'NONE', #2342, #4598 ) ;
#21910 = EDGE_CURVE ( 'NONE', #2574, #8091, #21575, .T. ) ;
#21911 = CARTESIAN_POINT ( 'NONE',  ( 139.5668999253178697, -3576.650121873226453, 2249.183459103710447 ) ) ;
#21912 = VERTEX_POINT ( 'NONE', #6860 ) ;
#21913 = DIRECTION ( 'NONE',  ( 0.000000000000000000, 0.000000000000000000, 1.000000000000000000 ) ) ;
#21914 = ORIENTED_EDGE ( 'NONE', *, *, #11576, .T. ) ;
#21915 = AXIS2_PLACEMENT_3D ( 'NONE', #9221, #4053, #21975 ) ;
#21916 = CARTESIAN_POINT ( 'NONE',  ( 12.42421805959000025, -3582.330875907999598, 2257.594929573999707 ) ) ;
#21917 = CARTESIAN_POINT ( 'NONE',  ( 15.24000000000000021, -3544.570000000000164, 2255.774000000000342 ) ) ;
#21918 = CIRCLE ( 'NONE', #7724, 5.460999999999938126 ) ;
#21919 = CIRCLE ( 'NONE', #21180, 1.269999999999882334 ) ;
#21920 = ORIENTED_EDGE ( 'NONE', *, *, #21839, .F. ) ;
#21921 = CARTESIAN_POINT ( 'NONE',  ( 12.70000000000000107, -3648.710000000000036, 2279.817639999999756 ) ) ;
#21922 = DIRECTION ( 'NONE',  ( 0.000000000000000000, 0.000000000000000000, -1.000000000000000000 ) ) ;
#21923 = ORIENTED_EDGE ( 'NONE', *, *, #17606, .F. ) ;
#21924 = DIRECTION ( 'NONE',  ( 0.000000000000000000, -1.000000000000000000, 0.000000000000000000 ) ) ;
#21925 = CARTESIAN_POINT ( 'NONE',  ( 14.13894186833527655, -3577.040487938397291, 2249.579033631703169 ) ) ;
#21926 = CARTESIAN_POINT ( 'NONE',  ( -0.7620000000000000107, -3660.140000000000327, 2243.785200000000259 ) ) ;
#21927 = EDGE_LOOP ( 'NONE', ( #6597, #15836, #13254, #21373 ) ) ;
#21928 = CARTESIAN_POINT ( 'NONE',  ( 139.5113228070520393, -3662.349796537330803, 2257.592643468492952 ) ) ;
#21929 = COORDINATED_UNIVERSAL_TIME_OFFSET ( 0, 0, .AHEAD. ) ;
#21930 = LINE ( 'NONE', #20513, #14876 ) ;
#21931 = CARTESIAN_POINT ( 'NONE',  ( 12.69999999999999929, -3639.502500000000055, 2288.971800000000258 ) ) ;
#21932 = LINE ( 'NONE', #5900, #9656 ) ;
#21933 = AXIS2_PLACEMENT_3D ( 'NONE', #10475, #12242, #22771 ) ;
#21934 = TOROIDAL_SURFACE ( 'NONE', #8826, 6.477000000001000402, 0.7620000000000000107 ) ;
#21935 = CARTESIAN_POINT ( 'NONE',  ( -12.69999999999999929, -3660.140000000000327, 2247.392000000000280 ) ) ;
#21936 = TOROIDAL_SURFACE ( 'NONE', #238, 3.606799999999999784, 0.7620000000000000107 ) ;
#21937 = ORIENTED_EDGE ( 'NONE', *, *, #10811, .T. ) ;
#21938 = CARTESIAN_POINT ( 'NONE',  ( 137.9195094541193214, -3661.723873492530402, 2249.755159743324384 ) ) ;
#21939 = APPLIED_PERSON_AND_ORGANIZATION_ASSIGNMENT ( #6349, #6237, ( #3730 ) ) ;
#21940 = ORIENTED_EDGE ( 'NONE', *, *, #3127, .T. ) ;
#21941 = CARTESIAN_POINT ( 'NONE',  ( 139.7000000001000046, -3656.812599999999748, 2239.391000000000076 ) ) ;
#21942 = LINE ( 'NONE', #15035, #21544 ) ;
#21943 = EDGE_CURVE ( 'NONE', #4269, #15765, #14002, .T. ) ;
#21944 = VERTEX_POINT ( 'NONE', #1570 ) ;
#21945 = PLANE ( 'NONE',  #18393 ) ;
#21946 = CARTESIAN_POINT ( 'NONE',  ( 35.56000000000000227, -3544.570000000000164, 2250.236800000000130 ) ) ;
#21947 = EDGE_CURVE ( 'NONE', #9977, #16048, #10337, .T. ) ;
#21948 = VERTEX_POINT ( 'NONE', #19153 ) ;
#21949 = AXIS2_PLACEMENT_3D ( 'NONE', #8311, #16857, #6212 ) ;
#21950 = CARTESIAN_POINT ( 'NONE',  ( 6.999092514601316317, -3659.102275462906164, 2244.742506506137033 ) ) ;
#21951 = LINE ( 'NONE', #21623, #4979 ) ;
#21952 = AXIS2_PLACEMENT_3D ( 'NONE', #7735, #11241, #7608 ) ;
#21953 = CARTESIAN_POINT ( 'NONE',  ( 116.8400000000000034, -3544.570000000000164, 2247.392000000000280 ) ) ;
#21954 = CALENDAR_DATE ( 2026, 26, 10 ) ;
#21955 = CIRCLE ( 'NONE', #11852, 0.7619999999999294005 ) ;
#21956 = DIRECTION ( 'NONE',  ( 0.000000000000000000, 0.000000000000000000, 1.000000000000000000 ) ) ;
#21957 = ORIENTED_EDGE ( 'NONE', *, *, #4147, .F. ) ;
#21958 = DIRECTION ( 'NONE',  ( 0.000000000000000000, 0.000000000000000000, 1.000000000000000000 ) ) ;
#21959 = DIRECTION ( 'NONE',  ( 0.000000000000000000, 0.000000000000000000, 1.000000000000000000 ) ) ;
#21960 = EDGE_LOOP ( 'NONE', ( #4621, #23133, #488, #4672, #4086, #12297, #5626, #2514 ) ) ;
#21961 = AXIS2_PLACEMENT_3D ( 'NONE', #7, #1873, #5398 ) ;
#21962 = FACE_OUTER_BOUND ( 'NONE', #9883, .T. ) ;
#21963 = APPLIED_DATE_AND_TIME_ASSIGNMENT ( #19049, #20923, ( #11226 ) ) ;
#21964 = CIRCLE ( 'NONE', #20462, 5.080000000000000959 ) ;
#21965 = DIRECTION ( 'NONE',  ( 1.000000000000000000, 0.000000000000000000, 0.000000000000000000 ) ) ;
#21966 = DIRECTION ( 'NONE',  ( 0.000000000000000000, 1.000000000000000000, 0.000000000000000000 ) ) ;
#21967 = CARTESIAN_POINT ( 'NONE',  ( 12.69999999994000106, -3636.810100000000148, 2292.781800000000203 ) ) ;
#21968 = VERTEX_POINT ( 'NONE', #3444 ) ;
#21969 = CARTESIAN_POINT ( 'NONE',  ( 7.020348529275000082, -3578.860230781999689, 2244.548186305999934 ) ) ;
#21970 = EDGE_CURVE ( 'NONE', #833, #5265, #22673, .T. ) ;
#21971 = AXIS2_PLACEMENT_3D ( 'NONE', #16125, #5589, #3695 ) ;
#21972 = EDGE_LOOP ( 'NONE', ( #12438, #20540, #17627, #15864, #3011, #8141, #19361, #10996, #8440, #107 ) ) ;
#21973 = DIRECTION ( 'NONE',  ( 0.000000000000000000, 0.000000000000000000, -1.000000000000000000 ) ) ;
#21974 = FACE_OUTER_BOUND ( 'NONE', #1948, .T. ) ;
#21975 = DIRECTION ( 'NONE',  ( 1.000000000000000000, 0.000000000000000000, 0.000000000000000000 ) ) ;
#21976 = EDGE_CURVE ( 'NONE', #9879, #13412, #17268, .T. ) ;
#21977 = CARTESIAN_POINT ( 'NONE',  ( -6.350000000000118661, -3660.140000000000327, 2242.311999999999898 ) ) ;
#21978 = CARTESIAN_POINT ( 'NONE',  ( 142.3712129903081518, -3543.717426572816294, 2255.445345401364193 ) ) ;
#21979 = CARTESIAN_POINT ( 'NONE',  ( 9.987313202991684236, -3657.938829547518253, 2239.009999999999764 ) ) ;
#21980 = CARTESIAN_POINT ( 'NONE',  ( 7.057989306600019219, -3578.573285425562972, 2244.557874998726220 ) ) ;
#21981 = ORIENTED_EDGE ( 'NONE', *, *, #20578, .F. ) ;
#21982 = CALENDAR_DATE ( 2026, 26, 10 ) ;
#21983 = AXIS2_PLACEMENT_3D ( 'NONE', #4458, #4350, #11596 ) ;
#21984 = CARTESIAN_POINT ( 'NONE',  ( 145.4149999979000256, -3659.390788570165569, 2244.645112239727041 ) ) ;
#21985 = EDGE_CURVE ( 'NONE', #4616, #8155, #17504, .T. ) ;
#21986 = AXIS2_PLACEMENT_3D ( 'NONE', #441, #14966, #3834 ) ;
#21987 = CARTESIAN_POINT ( 'NONE',  ( 9.887444566626168552, -3579.928195997985313, 2250.029480932760180 ) ) ;
#21988 = VECTOR ( 'NONE', #17220, 1000.000000000000000 ) ;
#21989 = DIRECTION ( 'NONE',  ( -2.318894227180156550E-14, -1.000000000000000000, 0.000000000000000000 ) ) ;
#21990 = EDGE_CURVE ( 'NONE', #21351, #2568, #6610, .T. ) ;
#21991 = ORIENTED_EDGE ( 'NONE', *, *, #10196, .T. ) ;
#21992 = DIRECTION ( 'NONE',  ( -1.000000000000000000, 0.000000000000000000, 0.000000000000000000 ) ) ;
#21993 = LINE ( 'NONE', #770, #2049 ) ;
#21994 = EDGE_LOOP ( 'NONE', ( #1879, #5178 ) ) ;
#21995 = PLANE ( 'NONE',  #11063 ) ;
#21996 = VECTOR ( 'NONE', #21191, 1000.000000000000000 ) ;
#21997 = DIRECTION ( 'NONE',  ( -1.000000000000000000, 0.000000000000000000, 0.000000000000000000 ) ) ;
#21998 = VERTEX_POINT ( 'NONE', #12118 ) ;
#21999 = CARTESIAN_POINT ( 'NONE',  ( 10.78733304872000076, -3657.399152860999493, 2246.630000000000109 ) ) ;
#22000 = DIRECTION ( 'NONE',  ( -1.000000000000000000, 0.000000000000000000, 0.000000000000000000 ) ) ;
#22001 = AXIS2_PLACEMENT_3D ( 'NONE', #7789, #9090, #7333 ) ;
#22002 = EDGE_CURVE ( 'NONE', #5746, #11629, #12216, .T. ) ;
#22003 = EDGE_LOOP ( 'NONE', ( #19357, #17517, #2266, #15676 ) ) ;
#22004 = DIRECTION ( 'NONE',  ( 0.000000000000000000, 0.000000000000000000, -1.000000000000000000 ) ) ;
#22005 = DIRECTION ( 'NONE',  ( 1.000000000000000000, 0.000000000000000000, 0.000000000000000000 ) ) ;
#22006 = VERTEX_POINT ( 'NONE', #12355 ) ;
#22007 = ADVANCED_FACE ( 'NONE', ( #17737 ), #19501, .F. ) ;
#22008 = EDGE_CURVE ( 'NONE', #13496, #17006, #12949, .T. ) ;
#22009 = DIRECTION ( 'NONE',  ( 0.000000000000000000, 0.000000000000000000, -1.000000000000000000 ) ) ;
#22010 = VERTEX_POINT ( 'NONE', #14236 ) ;
#22011 = CARTESIAN_POINT ( 'NONE',  ( 145.3179258180492752, -3580.544012085779286, 2245.098288301110188 ) ) ;
#22012 = PERSON_AND_ORGANIZATION ( #5446, #1895 ) ;
#22013 = CARTESIAN_POINT ( 'NONE',  ( 14.47433926966999884, -3641.733985386000313, 2279.676072425999791 ) ) ;
#22014 = CARTESIAN_POINT ( 'NONE',  ( 17.87993129502918777, -3661.919911407861491, 2245.171352655763712 ) ) ;
#22015 = EDGE_CURVE ( 'NONE', #4703, #15062, #1733, .T. ) ;
#22016 = CARTESIAN_POINT ( 'NONE',  ( 22.00181536726000076, -3544.061999999999898, 2275.224984633000076 ) ) ;
#22017 = CARTESIAN_POINT ( 'NONE',  ( 9.855200508358999301, -3579.494986006000545, 2257.962940201000038 ) ) ;
#22018 = CARTESIAN_POINT ( 'NONE',  ( 141.5164385476758753, -3577.305427569615858, 2249.774537136630897 ) ) ;
#22019 = ORIENTED_EDGE ( 'NONE', *, *, #22885, .F. ) ;
#22020 = EDGE_CURVE ( 'NONE', #20297, #118, #13771, .T. ) ;
#22021 = ORIENTED_EDGE ( 'NONE', *, *, #18248, .F. ) ;
#22022 = DIRECTION ( 'NONE',  ( 0.000000000000000000, 1.000000000000000000, 0.000000000000000000 ) ) ;
#22023 = ORIENTED_EDGE ( 'NONE', *, *, #11720, .T. ) ;
#22024 = CARTESIAN_POINT ( 'NONE',  ( 15.53320999718999929, -3599.183150532000127, 2279.450415100000100 ) ) ;
#22025 = DIRECTION ( 'NONE',  ( 0.000000000000000000, 0.000000000000000000, -1.000000000000000000 ) ) ;
#22026 = ORIENTED_EDGE ( 'NONE', *, *, #4987, .T. ) ;
#22027 = DIRECTION ( 'NONE',  ( -1.000000000000000000, 0.000000000000000000, 0.000000000000000000 ) ) ;
#22028 = AXIS2_PLACEMENT_3D ( 'NONE', #6081, #13209, #18603 ) ;
#22029 = VERTEX_POINT ( 'NONE', #21268 ) ;
#22030 = APPLICATION_CONTEXT ( 'configuration controlled 3d designs of mechanical parts and assemblies' ) ;
#22031 = DIRECTION ( 'NONE',  ( -3.370353031811000117E-12, 1.000000000000000000, 1.649417656553999895E-12 ) ) ;
#22032 = EDGE_CURVE ( 'NONE', #9684, #17959, #17814, .T. ) ;
#22033 = CARTESIAN_POINT ( 'NONE',  ( 14.37057332318734382, -3577.190483362103805, 2249.696470782429969 ) ) ;
#22034 =( NAMED_UNIT ( * ) SI_UNIT ( $, .STERADIAN. ) SOLID_ANGLE_UNIT ( ) );
#22035 = CARTESIAN_POINT ( 'NONE',  ( 142.0869831723413199, -3581.042548131108560, 2249.216657478487832 ) ) ;
#22036 = VERTEX_POINT ( 'NONE', #6742 ) ;
#22037 = DIRECTION ( 'NONE',  ( -1.000000000000000000, 0.000000000000000000, 0.000000000000000000 ) ) ;
#22038 = DATE_AND_TIME ( #18298, #2993 ) ;
#22039 = DIRECTION ( 'NONE',  ( 1.000000000000000000, 0.000000000000000000, 0.000000000000000000 ) ) ;
#22040 = CARTESIAN_POINT ( 'NONE',  ( 25.39999999999999858, -3660.140000000000327, 2247.392000000000280 ) ) ;
#22041 = CARTESIAN_POINT ( 'NONE',  ( 12.69999999999999929, -3570.287499999999909, 2257.592639999999847 ) ) ;
#22042 = AXIS2_PLACEMENT_3D ( 'NONE', #5344, #8512, #1703 ) ;
#22043 = DIRECTION ( 'NONE',  ( 0.000000000000000000, 0.000000000000000000, -1.000000000000000000 ) ) ;
#22044 = ORIENTED_EDGE ( 'NONE', *, *, #19094, .F. ) ;
#22045 = AXIS2_PLACEMENT_3D ( 'NONE', #22197, #11535, #9776 ) ;
#22046 = CARTESIAN_POINT ( 'NONE',  ( 140.2432324407819237, -3662.298289484956513, 2249.245429607616643 ) ) ;
#22047 = ADVANCED_FACE ( 'NONE', ( #21381 ), #6632, .T. ) ;
#22048 = ORIENTED_EDGE ( 'NONE', *, *, #18850, .T. ) ;
#22049 = VERTEX_POINT ( 'NONE', #8610 ) ;
#22050 = CARTESIAN_POINT ( 'NONE',  ( 15.41268679713999923, -3601.063670452857423, 2296.591799999999694 ) ) ;
#22051 = VERTEX_POINT ( 'NONE', #13882 ) ;
#22052 = CYLINDRICAL_SURFACE ( 'NONE', #9423, 5.460999999999938126 ) ;
#22053 = CARTESIAN_POINT ( 'NONE',  ( 139.6999999999999886, -3659.504999999999654, 2272.030000000000200 ) ) ;
#22054 = AXIS2_PLACEMENT_3D ( 'NONE', #22705, #13694, #1257 ) ;
#22055 = ORIENTED_EDGE ( 'NONE', *, *, #837, .T. ) ;
#22056 = DIRECTION ( 'NONE',  ( -1.000000000000000000, 0.000000000000000000, 0.000000000000000000 ) ) ;
#22057 = DIRECTION ( 'NONE',  ( 1.000000000000000000, 0.000000000000000000, 0.000000000000000000 ) ) ;
#22058 = DIRECTION ( 'NONE',  ( -4.702395060216999850E-14, -1.000000000000000000, 1.319970543219000025E-14 ) ) ;
#22059 = SECURITY_CLASSIFICATION ( '', '', #9651 ) ;
#22060 = AXIS2_PLACEMENT_3D ( 'NONE', #14357, #12598, #17867 ) ;
#22061 = FACE_OUTER_BOUND ( 'NONE', #4891, .T. ) ;
#22062 = DATE_AND_TIME ( #847, #22472 ) ;
#22063 = APPLIED_DATE_AND_TIME_ASSIGNMENT ( #19783, #3442, ( #10136 ) ) ;
#22064 =( REPRESENTATION_RELATIONSHIP ('NONE','NONE', #20448, #536 ) REPRESENTATION_RELATIONSHIP_WITH_TRANSFORMATION ( #1807 )SHAPE_REPRESENTATION_RELATIONSHIP( ) );
#22065 = DIRECTION ( 'NONE',  ( 0.000000000000000000, 0.000000000000000000, 1.000000000000000000 ) ) ;
#22066 = CARTESIAN_POINT ( 'NONE',  ( 144.3113860274000047, -3662.880847139000252, 2246.630000000000109 ) ) ;
#22067 = LINE ( 'NONE', #12608, #13765 ) ;
#22068 = ORIENTED_EDGE ( 'NONE', *, *, #3609, .F. ) ;
#22069 = B_SPLINE_CURVE_WITH_KNOTS ( 'NONE', 3,
 ( #3963, #10997, #7712, #21999 ),
 .UNSPECIFIED., .F., .F.,
 ( 4, 4 ),
 ( 0.000000000000000000, 1.000000000000000000 ),
 .UNSPECIFIED. ) ;
#22070 = FACE_OUTER_BOUND ( 'NONE', #6257, .T. ) ;
#22071 = CIRCLE ( 'NONE', #14247, 0.7619999999999294005 ) ;
#22072 = APPLIED_APPROVAL_ASSIGNMENT ( #11912, ( #10100 ) ) ;
#22073 = FACE_OUTER_BOUND ( 'NONE', #22410, .T. ) ;
#22074 = ORIENTED_EDGE ( 'NONE', *, *, #15512, .F. ) ;
#22075 = CARTESIAN_POINT ( 'NONE',  ( 139.6999999999999886, -3579.494999999999891, 2272.030000000000200 ) ) ;
#22076 = DIRECTION ( 'NONE',  ( 0.8660254037820102058, -0.5000000000042060799, 0.000000000000000000 ) ) ;
#22077 = VERTEX_POINT ( 'NONE', #19620 ) ;
#22078 = ORIENTED_EDGE ( 'NONE', *, *, #19872, .F. ) ;
#22079 = DIRECTION ( 'NONE',  ( 0.000000000000000000, 0.000000000000000000, -1.000000000000000000 ) ) ;
#22080 = DIRECTION ( 'NONE',  ( -1.000000000000000000, 2.318894227180000040E-14, 2.343004830739999973E-14 ) ) ;
#22081 =( BOUNDED_CURVE ( )  B_SPLINE_CURVE ( 3, ( #18225, #14495, #14720, #4048 ),
 .UNSPECIFIED., .F., .T. ) 
 B_SPLINE_CURVE_WITH_KNOTS ( ( 4, 4 ),
 ( 3.141592653589793116, 4.712388980572752573 ),
 .UNSPECIFIED. ) 
 CURVE ( )  GEOMETRIC_REPRESENTATION_ITEM ( )  RATIONAL_B_SPLINE_CURVE ( ( 1.000000000000000000, 0.8047378540800381730, 0.8047378540800381730, 1.000000000000000000 ) ) 
 REPRESENTATION_ITEM ( '' )  );
#22082 = PLANE ( 'NONE',  #9590 ) ;
#22083 = CARTESIAN_POINT ( 'NONE',  ( 10.36831320283000046, -3640.848700000000008, 2292.781800000000203 ) ) ;
#22084 = CARTESIAN_POINT ( 'NONE',  ( 116.8400000000000034, -3694.430000000000291, 2247.392000000000280 ) ) ;
#22085 = PLANE ( 'NONE',  #20325 ) ;
#22086 = CARTESIAN_POINT ( 'NONE',  ( -0.7620000000000000107, -3660.140000000000327, 2247.392000000000280 ) ) ;
#22087 = VERTEX_POINT ( 'NONE', #10123 ) ;
#22089 = AXIS2_PLACEMENT_3D ( 'NONE', #6322, #13455, #2784 ) ;
#22088 = CALENDAR_DATE ( 2026, 26, 10 ) ;
#22090 = APPLIED_DATE_AND_TIME_ASSIGNMENT ( #23128, #11062, ( #20962 ) ) ;
#22091 = CARTESIAN_POINT ( 'NONE',  ( -12.69999999999988027, -3660.140000000000327, 2252.472000000000207 ) ) ;
#22092 = LOCAL_TIME ( 17, 37, 43.00000000000000000, #1871 ) ;
#22093 = LOCAL_TIME ( 17, 37, 43.00000000000000000, #11317 ) ;
#22094 = CARTESIAN_POINT ( 'NONE',  ( 9.915707903441028037, -3580.080243487859207, 2249.961828650349162 ) ) ;
#22095 = CIRCLE ( 'NONE', #11996, 0.7619999999999294005 ) ;
#22096 = EDGE_CURVE ( 'NONE', #22077, #8967, #20810, .T. ) ;
#22097 = FACE_OUTER_BOUND ( 'NONE', #19397, .T. ) ;
#22098 = EDGE_CURVE ( 'NONE', #18111, #2160, #20914, .T. ) ;
#22099 = ORIENTED_EDGE ( 'NONE', *, *, #9764, .T. ) ;
#22100 = LINE ( 'NONE', #2205, #2902 ) ;
#22101 = ADVANCED_FACE ( 'NONE', ( #12592 ), #54, .F. ) ;
#22102 = ORIENTED_EDGE ( 'NONE', *, *, #10063, .F. ) ;
#22103 = CARTESIAN_POINT ( 'NONE',  ( 9.855190710340998805, -3579.495000415000050, 2250.165025612000136 ) ) ;
#22104 = CARTESIAN_POINT ( 'NONE',  ( 13.37322708549078065, -3662.269940902608596, 2249.277995755860502 ) ) ;
#22105 = FACE_OUTER_BOUND ( 'NONE', #15373, .T. ) ;
#22106 = ORIENTED_EDGE ( 'NONE', *, *, #9724, .F. ) ;
#22107 = ADVANCED_FACE ( 'NONE', ( #3676 ), #19854, .T. ) ;
#22108 = ORGANIZATION ( 'NAUO-ORG9', 'UNSPECIFIED', 'UNSPECIFIED' ) ;
#22109 = DIRECTION ( 'NONE',  ( 1.000000000000000000, 0.000000000000000000, 0.000000000000000000 ) ) ;
#22110 = APPROVAL_PERSON_ORGANIZATION ( #2876, #18237, #17162 ) ;
#22111 = DIRECTION ( 'NONE',  ( 1.000000000000000000, 0.000000000000000000, 0.000000000000000000 ) ) ;
#22112 = ORIENTED_EDGE ( 'NONE', *, *, #22969, .F. ) ;
#22113 = FACE_OUTER_BOUND ( 'NONE', #6016, .T. ) ;
#22114 = DIRECTION ( 'NONE',  ( 0.000000000000000000, 0.000000000000000000, -1.000000000000000000 ) ) ;
#22115 = ADVANCED_FACE ( 'NONE', ( #5447 ), #15298, .T. ) ;
#22116 = ORIENTED_EDGE ( 'NONE', *, *, #620, .T. ) ;
#22117 = AXIS2_PLACEMENT_3D ( 'NONE', #20925, #19401, #13895 ) ;
#22118 = EDGE_LOOP ( 'NONE', ( #13040, #9111, #5769, #15589 ) ) ;
#22119 = CIRCLE ( 'NONE', #14277, 5.460999999999938126 ) ;
#22120 = UNCERTAINTY_MEASURE_WITH_UNIT (LENGTH_MEASURE( 1.000000000000000082E-05 ), #7866, 'distance_accuracy_value', 'NONE');
#22121 = ORIENTED_EDGE ( 'NONE', *, *, #12670, .T. ) ;
#22122 = CARTESIAN_POINT ( 'NONE',  ( 145.0727138887509398, -3581.449656632165443, 2246.178647461291348 ) ) ;
#22123 = DATE_AND_TIME ( #7490, #7496 ) ;
#22124 = CARTESIAN_POINT ( 'NONE',  ( 145.3795747169000094, -3578.859731361000286, 2244.547525601999951 ) ) ;
#22125 = CARTESIAN_POINT ( 'NONE',  ( 18.21227314848903944, -3661.013619535250200, 2244.684649758042724 ) ) ;
#22126 = EDGE_CURVE ( 'NONE', #11962, #7810, #4361, .T. ) ;
#22127 = CARTESIAN_POINT ( 'NONE',  ( 79.80679999999999552, -3568.700000000000273, 2259.837999999999738 ) ) ;
#22128 = ADVANCED_FACE ( 'NONE', ( #1922 ), #2946, .T. ) ;
#22129 = CARTESIAN_POINT ( 'NONE',  ( 137.7151180025381336, -3577.456461149886763, 2249.866723821840424 ) ) ;
#22130 = EDGE_LOOP ( 'NONE', ( #16331, #16520, #230, #14747 ) ) ;
#22131 = CIRCLE ( 'NONE', #10550, 0.7619999999999294005 ) ;
#22132 = DIRECTION ( 'NONE',  ( 0.000000000000000000, -1.000000000000000000, 0.000000000000000000 ) ) ;
#22133 = CIRCLE ( 'NONE', #19897, 2.844799999998931295 ) ;
#22134 = DIRECTION ( 'NONE',  ( 1.000000000000000000, 0.000000000000000000, 0.000000000000000000 ) ) ;
#22135 = ORIENTED_EDGE ( 'NONE', *, *, #21851, .T. ) ;
#22136 = CARTESIAN_POINT ( 'NONE',  ( 18.37893127878000143, -3660.140301727999940, 2244.547200027999679 ) ) ;
#22137 = DIRECTION ( 'NONE',  ( 0.000000000000000000, 0.000000000000000000, -1.000000000000000000 ) ) ;
#22138 = VERTEX_POINT ( 'NONE', #16105 ) ;
#22139 = ORIENTED_EDGE ( 'NONE', *, *, #10361, .F. ) ;
#22140 = ORIENTED_EDGE ( 'NONE', *, *, #21976, .T. ) ;
#22141 = CARTESIAN_POINT ( 'NONE',  ( 101.5999999999999943, -3619.500000000000000, 2260.600000000000364 ) ) ;
#22142 = EDGE_LOOP ( 'NONE', ( #5245, #9832, #12107, #3534 ) ) ;
#22143 = DIRECTION ( 'NONE',  ( 0.000000000000000000, 0.000000000000000000, 1.000000000000000000 ) ) ;
#22144 = CARTESIAN_POINT ( 'NONE',  ( 14.17803026764341467, -3577.063814636674124, 2249.598259528346262 ) ) ;
#22145 = CARTESIAN_POINT ( 'NONE',  ( 142.4822567032824452, -3580.090015056482571, 2249.957167306039082 ) ) ;
#22146 = ORIENTED_EDGE ( 'NONE', *, *, #4364, .T. ) ;
#22148 = CARTESIAN_POINT ( 'NONE',  ( 138.4354735356341735, -3662.060017425506430, 2257.663486769918109 ) ) ;
#22147 = VECTOR ( 'NONE', #13139, 1000.000000000000227 ) ;
#22149 = PERSON_AND_ORGANIZATION_ROLE ( 'creator' ) ;
#22150 = CIRCLE ( 'NONE', #1961, 2.844800000000091700 ) ;
#22151 = CARTESIAN_POINT ( 'NONE',  ( 12.69999999999999929, -3579.494999999999891, 2239.771999999999935 ) ) ;
#22152 = DIRECTION ( 'NONE',  ( -1.224646799147353207E-16, 1.000000000000000000, 0.000000000000000000 ) ) ;
#22153 = CARTESIAN_POINT ( 'NONE',  ( 139.6999999999999886, -3659.504999999999654, 2246.630000000000109 ) ) ;
#22154 = VERTEX_POINT ( 'NONE', #8958 ) ;
#22155 = CIRCLE ( 'NONE', #4205, 3.606799999999993567 ) ;
#22156 = CARTESIAN_POINT ( 'NONE',  ( -12.69999999999666507, -3577.422685254746739, 2244.902497835742906 ) ) ;
#22157 = EDGE_CURVE ( 'NONE', #14295, #7706, #7201, .T. ) ;
#22158 = EDGE_CURVE ( 'NONE', #17044, #18172, #22387, .T. ) ;
#22159 = EDGE_LOOP ( 'NONE', ( #4222, #11473, #2332, #21441, #23014 ) ) ;
#22160 = EDGE_CURVE ( 'NONE', #12867, #11171, #2105, .T. ) ;
#22161 = VECTOR ( 'NONE', #22226, 1000.000000000000000 ) ;
#22162 = ORIENTED_EDGE ( 'NONE', *, *, #18697, .F. ) ;
#22163 = AXIS2_PLACEMENT_3D ( 'NONE', #16953, #783, #11454 ) ;
#22164 = DIRECTION ( 'NONE',  ( -1.000000000000000000, 0.000000000000000000, 0.000000000000000000 ) ) ;
#22165 = ORIENTED_EDGE ( 'NONE', *, *, #4677, .T. ) ;
#22166 = PLANE ( 'NONE',  #1171 ) ;
#22167 = DIRECTION ( 'NONE',  ( 1.000000000000000000, 0.000000000000000000, 0.000000000000000000 ) ) ;
#22168 = EDGE_CURVE ( 'NONE', #21153, #13850, #7728, .T. ) ;
#22169 = ORIENTED_EDGE ( 'NONE', *, *, #4065, .F. ) ;
#22170 = AXIS2_PLACEMENT_3D ( 'NONE', #20345, #11766, #7809 ) ;
#22171 = CYLINDRICAL_SURFACE ( 'NONE', #4721, 1.269999999999882334 ) ;
#22172 = DIRECTION ( 'NONE',  ( 0.000000000000000000, 0.000000000000000000, 1.000000000000000000 ) ) ;
#22173 = CYLINDRICAL_SURFACE ( 'NONE', #2378, 1.269999999999993356 ) ;
#22174 = DIRECTION ( 'NONE',  ( -0.8660254037840939834, -0.5000000000005969669, 0.000000000000000000 ) ) ;
#22175 = AXIS2_PLACEMENT_3D ( 'NONE', #20431, #18329, #853 ) ;
#22176 = ADVANCED_FACE ( 'NONE', ( #5513 ), #16500, .T. ) ;
#22177 = PERSON_AND_ORGANIZATION ( #5446, #1895 ) ;
#22178 = ADVANCED_FACE ( 'NONE', ( #2217 ), #23143, .T. ) ;
#22179 = CARTESIAN_POINT ( 'NONE',  ( 3.810000000000000053, -3544.061999999999898, 2238.248000000000047 ) ) ;
#22180 = TOROIDAL_SURFACE ( 'NONE', #10970, 5.080000000000000071, 0.3810000000000000053 ) ;
#22181 = DIRECTION ( 'NONE',  ( 0.7071067811864976127, 0.000000000000000000, -0.7071067811865975328 ) ) ;
#22182 = ORIENTED_EDGE ( 'NONE', *, *, #22517, .T. ) ;
#22183 = CARTESIAN_POINT ( 'NONE',  ( 9.926985991717000246, -3578.860012824000023, 2250.236835079999764 ) ) ;
#22184 = CARTESIAN_POINT ( 'NONE',  ( 0.000000000000000000, -3544.570000000000164, 2259.329999999999927 ) ) ;
#22185 = ADVANCED_BREP_SHAPE_REPRESENTATION ( '', ( #6253, #5611 ), #6759 ) ;
#22186 = ORIENTED_EDGE ( 'NONE', *, *, #5008, .T. ) ;
#22187 = AXIS2_PLACEMENT_3D ( 'NONE', #19698, #5636, #12771 ) ;
#22188 = DIRECTION ( 'NONE',  ( -1.000000000000000000, 0.000000000000000000, 0.000000000000000000 ) ) ;
#22189 = DIRECTION ( 'NONE',  ( 0.000000000000000000, 0.000000000000000000, -1.000000000000000000 ) ) ;
#22190 = VERTEX_POINT ( 'NONE', #3615 ) ;
#22191 = ORIENTED_EDGE ( 'NONE', *, *, #10784, .T. ) ;
#22192 = CARTESIAN_POINT ( 'NONE',  ( 25.39999999999999858, -3660.140000000000327, 2250.236800000000130 ) ) ;
#22193 = CARTESIAN_POINT ( 'NONE',  ( 12.69999999999999929, -3576.650200000000041, 2257.592639999999847 ) ) ;
#22194 = CIRCLE ( 'NONE', #8364, 5.080000000000000959 ) ;
#22195 = CARTESIAN_POINT ( 'NONE',  ( 0.000000000000000000, -3578.860000000000127, 2247.392000000000280 ) ) ;
#22196 = VECTOR ( 'NONE', #8342, 1000.000000000000000 ) ;
#22197 = CARTESIAN_POINT ( 'NONE',  ( -6.349999999999999645, -3660.140000000000327, 2247.392000000000280 ) ) ;
#22198 = DIRECTION ( 'NONE',  ( 0.000000000000000000, 0.000000000000000000, 1.000000000000000000 ) ) ;
#22199 = PLANE ( 'NONE',  #8716 ) ;
#22200 = LINE ( 'NONE', #18802, #8336 ) ;
#22201 = VERTEX_POINT ( 'NONE', #5266 ) ;
#22202 = PERSON_AND_ORGANIZATION ( #5446, #1895 ) ;
#22203 = CARTESIAN_POINT ( 'NONE',  ( 9.855200508393229697, -3659.504999998446692, 2257.962940200992307 ) ) ;
#22204 = VECTOR ( 'NONE', #13956, 1000.000000000000000 ) ;
#22205 = CYLINDRICAL_SURFACE ( 'NONE', #3450, 2.844799999999999773 ) ;
#22206 = CARTESIAN_POINT ( 'NONE',  ( 91.74479999999999791, -3594.099999999999909, 2239.771999999999935 ) ) ;
#22207 = ORIENTED_EDGE ( 'NONE', *, *, #14838, .T. ) ;
#22208 = FACE_OUTER_BOUND ( 'NONE', #16888, .T. ) ;
#22209 = DIRECTION ( 'NONE',  ( 0.8660254037820102058, -0.5000000000042060799, 0.000000000000000000 ) ) ;
#22210 = DIRECTION ( 'NONE',  ( 0.000000000000000000, 1.000000000000000000, 0.000000000000000000 ) ) ;
#22211 = VERTEX_POINT ( 'NONE', #21326 ) ;
#22212 = CARTESIAN_POINT ( 'NONE',  ( 15.47299515201000020, -3578.859991782000179, 2250.236800948000109 ) ) ;
#22213 = DIRECTION ( 'NONE',  ( 0.000000000000000000, 0.000000000000000000, -1.000000000000000000 ) ) ;
#22214 = APPLIED_PERSON_AND_ORGANIZATION_ASSIGNMENT ( #576, #18267, ( #10864 ) ) ;
#22215 = CARTESIAN_POINT ( 'NONE',  ( 12.69999999999999929, -3599.497499999999945, 2296.210799999999836 ) ) ;
#22216 = ORIENTED_EDGE ( 'NONE', *, *, #8387, .F. ) ;
#22217 = CYLINDRICAL_SURFACE ( 'NONE', #14437, 11.11249999999985860 ) ;
#22218 = PLANE ( 'NONE',  #11435 ) ;
#22219 = ADVANCED_FACE ( 'NONE', ( #11001 ), #2563, .T. ) ;
#22220 = CARTESIAN_POINT ( 'NONE',  ( -0.7620000000000000107, -3578.860000000000127, 2243.785200000000259 ) ) ;
#22221 = CIRCLE ( 'NONE', #8393, 5.080000000000000959 ) ;
#22222 = CARTESIAN_POINT ( 'NONE',  ( 139.6999999999999886, -3570.287499999999909, 2268.705139999999574 ) ) ;
#22223 = ORIENTED_EDGE ( 'NONE', *, *, #7072, .T. ) ;
#22224 = ORIENTED_EDGE ( 'NONE', *, *, #11975, .T. ) ;
#22225 = ADVANCED_FACE ( 'NONE', ( #17797 ), #10770, .F. ) ;
#22226 = DIRECTION ( 'NONE',  ( 0.000000000000000000, 0.000000000000000000, -1.000000000000000000 ) ) ;
#22227 = ORIENTED_EDGE ( 'NONE', *, *, #17307, .T. ) ;
#22228 = CARTESIAN_POINT ( 'NONE',  ( 145.2068972130955160, -3581.023318633427607, 2245.544194199756021 ) ) ;
#22229 = DATE_AND_TIME ( #1254, #21722 ) ;
#22230 = CARTESIAN_POINT ( 'NONE',  ( 139.8886776217523220, -3576.650200000001405, 2257.592640000000301 ) ) ;
#22231 = CARTESIAN_POINT ( 'NONE',  ( 17.31138602737999932, -3662.880847139000252, 2246.630000000000109 ) ) ;
#22232 = CIRCLE ( 'NONE', #17002, 3.175000000000149925 ) ;
#22233 = PLANE ( 'NONE',  #14859 ) ;
#22234 = CIRCLE ( 'NONE', #6924, 5.080000000000000071 ) ;
#22235 = CARTESIAN_POINT ( 'NONE',  ( 142.0316867972038608, -3580.841200000134904, 2239.167815367294224 ) ) ;
#22236 = AXIS2_PLACEMENT_3D ( 'NONE', #1331, #6508, #6859 ) ;
#22237 = DIRECTION ( 'NONE',  ( -1.000000000000000000, 0.000000000000000000, 0.000000000000000000 ) ) ;
#22238 = ORIENTED_EDGE ( 'NONE', *, *, #20236, .F. ) ;
#22239 = CYLINDRICAL_SURFACE ( 'NONE', #17819, 11.11249999999985860 ) ;
#22240 = CARTESIAN_POINT ( 'NONE',  ( 57.15000000000030411, -3568.700000000000273, 2250.236800000000130 ) ) ;
#22241 = ORIENTED_EDGE ( 'NONE', *, *, #12730, .T. ) ;
#22242 = DIRECTION ( 'NONE',  ( 0.000000000000000000, -1.000000000000000000, 0.000000000000000000 ) ) ;
#22243 = VERTEX_POINT ( 'NONE', #10491 ) ;
#22244 = ADVANCED_FACE ( 'NONE', ( #9015, #5389 ), #7144, .F. ) ;
#22245 = ORIENTED_EDGE ( 'NONE', *, *, #21897, .T. ) ;
#22246 = DIRECTION ( 'NONE',  ( 0.000000000000000000, 0.000000000000000000, -1.000000000000000000 ) ) ;
#22247 = EDGE_CURVE ( 'NONE', #14198, #5555, #8188, .T. ) ;
#22248 = AXIS2_PLACEMENT_3D ( 'NONE', #10935, #14694, #7535 ) ;
#22249 = VECTOR ( 'NONE', #2402, 1000.000000000000000 ) ;
#22250 = EDGE_CURVE ( 'NONE', #16889, #16025, #13815, .T. ) ;
#22251 = ORIENTED_EDGE ( 'NONE', *, *, #17519, .F. ) ;
#22253 = EDGE_CURVE ( 'NONE', #2462, #18263, #20362, .T. ) ;
#22252 = AXIS2_PLACEMENT_3D ( 'NONE', #8434, #6687, #13825 ) ;
#22254 = LINE ( 'NONE', #20394, #13698 ) ;
#22255 = CARTESIAN_POINT ( 'NONE',  ( 11.46140658660981693, -3576.933588766896719, 2249.485458673201265 ) ) ;
#22256 = TOROIDAL_SURFACE ( 'NONE', #20396, 5.080000000000000071, 0.3810000000000000053 ) ;
#22257 = CARTESIAN_POINT ( 'NONE',  ( 142.0110375026553129, -3581.154241066639315, 2249.074962378318560 ) ) ;
#22258 = ORIENTED_EDGE ( 'NONE', *, *, #4855, .F. ) ;
#22259 = DIRECTION ( 'NONE',  ( -0.000000000000000000, 1.000000000000000000, 0.000000000000000000 ) ) ;
#22260 = PRODUCT_CONTEXT ( 'NONE', #1993, 'mechanical' ) ;
#22261 = EDGE_LOOP ( 'NONE', ( #20480, #17439, #9294, #20033 ) ) ;
#22262 = CARTESIAN_POINT ( 'NONE',  ( 20.60974739964567348, -3543.420597440594065, 2259.874498643110655 ) ) ;
#22263 = CARTESIAN_POINT ( 'NONE',  ( 12.69999999999999929, -3655.060000000000400, 2275.055139999999483 ) ) ;
#22264 = CIRCLE ( 'NONE', #14432, 0.7619999999999987894 ) ;
#22265 = ORIENTED_EDGE ( 'NONE', *, *, #17557, .F. ) ;
#22266 = VECTOR ( 'NONE', #6909, 1000.000000000000000 ) ;
#22267 = CARTESIAN_POINT ( 'NONE',  ( 19.05000000000000071, -3660.140000000000327, 2247.392000000000280 ) ) ;
#22268 = CIRCLE ( 'NONE', #7329, 5.460999999999938126 ) ;
#22269 = ORIENTED_EDGE ( 'NONE', *, *, #8235, .T. ) ;
#22270 = ORIENTED_EDGE ( 'NONE', *, *, #8662, .F. ) ;
#22271 = VECTOR ( 'NONE', #20752, 1000.000000000000000 ) ;
#22272 = DIRECTION ( 'NONE',  ( 0.000000000000000000, 0.000000000000000000, -1.000000000000000000 ) ) ;
#22273 = ORIENTED_EDGE ( 'NONE', *, *, #18787, .F. ) ;
#22274 = DIRECTION ( 'NONE',  ( -1.000000000000000000, 0.000000000000000000, 0.000000000000000000 ) ) ;
#22275 = DIRECTION ( 'NONE',  ( 0.000000000000000000, 0.000000000000000000, 1.000000000000000000 ) ) ;
#22276 = ORIENTED_EDGE ( 'NONE', *, *, #21947, .F. ) ;
#22277 = ADVANCED_FACE ( 'NONE', ( #9472 ), #11185, .T. ) ;
#22278 = DIRECTION ( 'NONE',  ( 2.324635735433000053E-14, 0.000000000000000000, 1.000000000000000000 ) ) ;
#22279 = CARTESIAN_POINT ( 'NONE',  ( 12.69999999999999929, -3599.497499999999945, 2290.622800000000097 ) ) ;
#22280 = CIRCLE ( 'NONE', #11803, 2.844800000000001550 ) ;
#22281 = VECTOR ( 'NONE', #532, 1000.000000000000000 ) ;
#22282 = DIRECTION ( 'NONE',  ( 0.000000000000000000, -1.000000000000000000, 0.000000000000000000 ) ) ;
#22283 = APPLICATION_PROTOCOL_DEFINITION ( 'international standard', 'automotive_design', 2000, #5277 ) ;
#22284 = EDGE_CURVE ( 'NONE', #15874, #21686, #7443, .T. ) ;
#22285 = AXIS2_PLACEMENT_3D ( 'NONE', #10243, #12357, #23006 ) ;
#22286 = ADVANCED_FACE ( 'NONE', ( #22338 ), #4313, .F. ) ;
#22287 = DIRECTION ( 'NONE',  ( 0.000000000000000000, 0.000000000000000000, -1.000000000000000000 ) ) ;
#22288 = CARTESIAN_POINT ( 'NONE',  ( 12.69999999999999929, -3648.710000000000036, 2268.705139999999574 ) ) ;
#22289 = VECTOR ( 'NONE', #17757, 1000.000000000000114 ) ;
#22290 = DIRECTION ( 'NONE',  ( 1.710167014410000085E-12, -1.000000000000000000, 0.000000000000000000 ) ) ;
#22291 = DIRECTION ( 'NONE',  ( -0.000000000000000000, -1.000000000000000000, -0.000000000000000000 ) ) ;
#22292 = TOROIDAL_SURFACE ( 'NONE', #20485, 5.080000000000000071, 0.3810000000000000053 ) ;
#22293 = CIRCLE ( 'NONE', #18197, 2.844799999999999773 ) ;
#22294 = EDGE_CURVE ( 'NONE', #1232, #17616, #4074, .T. ) ;
#22295 = VERTEX_POINT ( 'NONE', #16614 ) ;
#22296 = DIRECTION ( 'NONE',  ( -1.000000000000000000, 0.000000000000000000, 0.000000000000000000 ) ) ;
#22297 = AXIS2_PLACEMENT_3D ( 'NONE', #22664, #8383, #15764 ) ;
#22298 = VERTEX_POINT ( 'NONE', #782 ) ;
#22299 = EDGE_CURVE ( 'NONE', #3849, #8091, #17159, .T. ) ;
#22300 = DIRECTION ( 'NONE',  ( 1.000000000000000000, 0.000000000000000000, 0.000000000000000000 ) ) ;
#22301 = PRODUCT_DEFINITION_SHAPE ( 'NONE', 'NONE',  #23176 ) ;
#22302 = CIRCLE ( 'NONE', #20442, 0.7620000000000366480 ) ;
#22303 = EDGE_CURVE ( 'NONE', #6778, #10158, #9688, .T. ) ;
#22304 = CARTESIAN_POINT ( 'NONE',  ( 101.5999999999999943, -3670.300000000000182, 2260.600000000000364 ) ) ;
#22305 = ORIENTED_EDGE ( 'NONE', *, *, #63, .T. ) ;
#22306 = VERTEX_POINT ( 'NONE', #14979 ) ;
#22307 = SPHERICAL_SURFACE ( 'NONE', #3405, 0.7620000000000000107 ) ;
#22308 = CARTESIAN_POINT ( 'NONE',  ( 7.619999999999999218, -3579.494999999999891, 2245.359999999999673 ) ) ;
#22309 = AXIS2_PLACEMENT_3D ( 'NONE', #2059, #20213, #14489 ) ;
#22310 = DIRECTION ( 'NONE',  ( 1.148603104910000072E-12, 1.000000000000000000, 0.000000000000000000 ) ) ;
#22311 = DIRECTION ( 'NONE',  ( -1.000000000000000000, 0.000000000000000000, 0.000000000000000000 ) ) ;
#22312 = CARTESIAN_POINT ( 'NONE',  ( 142.4730239663999782, -3578.859999866000180, 2250.236800057000437 ) ) ;
#22313 = ORIENTED_EDGE ( 'NONE', *, *, #16655, .F. ) ;
#22314 = PERSON_AND_ORGANIZATION ( #5446, #1895 ) ;
#22315 = EDGE_CURVE ( 'NONE', #9475, #15597, #12309, .T. ) ;
#22316 = ORIENTED_EDGE ( 'NONE', *, *, #7142, .F. ) ;
#22317 = DIRECTION ( 'NONE',  ( 0.000000000000000000, 1.000000000000000000, 0.000000000000000000 ) ) ;
#22318 = VERTEX_POINT ( 'NONE', #20478 ) ;
#22319 = VECTOR ( 'NONE', #13482, 1000.000000000000000 ) ;
#22320 = DIRECTION ( 'NONE',  ( 4.128125857098999856E-13, -1.295098308108999758E-13, -1.000000000000000000 ) ) ;
#22321 = AXIS2_PLACEMENT_3D ( 'NONE', #20644, #11292, #632 ) ;
#22322 = CARTESIAN_POINT ( 'NONE',  ( 12.69999999999999929, -3579.494999999999891, 2270.760000000000218 ) ) ;
#22323 = AXIS2_PLACEMENT_3D ( 'NONE', #2564, #9710, #20490 ) ;
#22324 = EDGE_LOOP ( 'NONE', ( #22910, #13932 ) ) ;
#22325 = CARTESIAN_POINT ( 'NONE',  ( 12.69999999999999929, -3581.400000000000091, 2272.030000000000200 ) ) ;
#22326 = CIRCLE ( 'NONE', #5142, 1.269999999999882334 ) ;
#22327 = DIRECTION ( 'NONE',  ( 0.000000000000000000, 0.000000000000000000, 1.000000000000000000 ) ) ;
#22328 = CARTESIAN_POINT ( 'NONE',  ( 145.3724401638749839, -3660.201886162340543, 2244.547775376675872 ) ) ;
#22329 = ORIENTED_EDGE ( 'NONE', *, *, #468, .T. ) ;
#22330 = DIRECTION ( 'NONE',  ( 0.000000000000000000, -1.000000000000000000, 0.000000000000000000 ) ) ;
#22331 = EDGE_CURVE ( 'NONE', #4775, #10874, #13060, .T. ) ;
#22332 = CARTESIAN_POINT ( 'NONE',  ( -12.31900000000000084, -3660.140000000000327, 2247.392000000000280 ) ) ;
#22333 = CARTESIAN_POINT ( 'NONE',  ( -8.890000000008999592, -3662.832400000000234, 2247.392000000000280 ) ) ;
#22334 = ORIENTED_EDGE ( 'NONE', *, *, #8356, .T. ) ;
#22335 = LINE ( 'NONE', #2893, #13671 ) ;
#22336 = CARTESIAN_POINT ( 'NONE',  ( -12.69999999999999929, -3658.573829547000059, 2244.679313203000220 ) ) ;
#22337 = CIRCLE ( 'NONE', #5908, 2.844800000000091700 ) ;
#22338 = FACE_OUTER_BOUND ( 'NONE', #13293, .T. ) ;
#22339 = CARTESIAN_POINT ( 'NONE',  ( 136.6540434515666504, -3581.600851036878794, 2246.630014020016006 ) ) ;
#22340 = CARTESIAN_POINT ( 'NONE',  ( -12.69999999999997442, -3657.007659094873816, 2247.391999999781547 ) ) ;
#22341 = VERTEX_POINT ( 'NONE', #18373 ) ;
#22342 = CIRCLE ( 'NONE', #15626, 1.240967364599221412 ) ;
#22343 = VECTOR ( 'NONE', #19953, 1000.000000000000000 ) ;
#22344 = LINE ( 'NONE', #18713, #21044 ) ;
#22345 = EDGE_LOOP ( 'NONE', ( #21029, #7486, #9919, #15980, #13392, #748 ) ) ;
#22346 = B_SPLINE_CURVE_WITH_KNOTS ( 'NONE', 3,
 ( #16627, #5875, #4098, #18274, #11015, #584, #5981, #16177, #14424, #5530, #9268, #7738, #128, #13013, #12772, #7273, #12659, #18159, #21576, #469, #14890, #22018, #11244, #20049, #13119, #5639, #1999, #7610, #9379, #14545, #20272, #4214, #17924, #1878, #3985, #16404, #3743, #11136, #18390, #21911, #9030, #10900, #9488, #21681, #7392, #16513, #19812, #20160, #2344, #356, #14771, #14656, #7497, #18049, #19928, #9149, #21797, #16290, #251, #5758, #12892, #6100, #20719, #22129, #2461, #6561, #15110, #14996, #13699, #2914, #20601, #795, #17199, #11352, #1145, #2567, #16970, #10054 ),
 .UNSPECIFIED., .F., .F.,
 ( 4, 2, 2, 1, 2, 2, 2, 1, 2, 2, 2, 1, 2, 2, 2, 2, 2, 2, 1, 2, 2, 2, 2, 2, 1, 2, 2, 2, 2, 2, 2, 1, 2, 2, 2, 1, 2, 2, 2, 1, 2, 2, 4 ),
 ( 0.000000000000000000, 0.06249999999892112690, 0.09374999999839656040, 0.1093749999981342841, 0.1171874999980031529, 0.1249999999978720078, 0.1562499999974240328, 0.1718749999971419806, 0.1796874999969980680, 0.1874999999968541553, 0.2187499999964742092, 0.2343749999963266051, 0.2421874999962923825, 0.2499999999962581598, 0.2812499999963358199, 0.2968749999963781194, 0.3124999999964203634, 0.3437499999965609732, 0.3593749999966041053, 0.3671874999966006636, 0.3749999999965971664, 0.4999999999971623810, 0.5624999999974512610, 0.5937499999976098009, 0.6093749999976889598, 0.6171874999977259302, 0.6249999999977630116, 0.6562499999977361442, 0.6718749999976957321, 0.6874999999976552090, 0.7187499999976278975, 0.7343749999976073584, 0.7421874999976002529, 0.7499999999975931475, 0.7812499999979156673, 0.7968749999980019316, 0.8046874999980959675, 0.8124999999981898924, 0.8437499999986749488, 0.8593749999989175326, 0.8671874999990610844, 0.8749999999992046362, 1.000000000000000000 ),
 .UNSPECIFIED. ) ;
#22347 = CARTESIAN_POINT ( 'NONE',  ( 145.1333241165027630, -3581.267160291652999, 2245.875868943096521 ) ) ;
#22348 = DATE_AND_TIME ( #4894, #21737 ) ;
#22349 = APPLIED_DATE_AND_TIME_ASSIGNMENT ( #20711, #4658, ( #6021 ) ) ;
#22350 = CARTESIAN_POINT ( 'NONE',  ( 141.4511983633885279, -3577.222884639119002, 2257.728283138646020 ) ) ;
#22351 = DIRECTION ( 'NONE',  ( 0.000000000000000000, 0.000000000000000000, 1.000000000000000000 ) ) ;
#22352 = DIRECTION ( 'NONE',  ( 0.000000000000000000, 1.000000000000000000, 0.000000000000000000 ) ) ;
#22353 = CARTESIAN_POINT ( 'NONE',  ( 40.94480000000000075, -3594.099999999999909, 2259.837999999999738 ) ) ;
#22354 = AXIS2_PLACEMENT_3D ( 'NONE', #14510, #5250, #16142 ) ;
#22355 = CARTESIAN_POINT ( 'NONE',  ( 139.7000000001000046, -3656.812599999999748, 2242.820000000000164 ) ) ;
#22356 = ORIENTED_EDGE ( 'NONE', *, *, #14571, .T. ) ;
#22357 = B_SPLINE_CURVE_WITH_KNOTS ( 'NONE', 3,
 ( #9913, #20579, #17062, #11795 ),
 .UNSPECIFIED., .F., .F.,
 ( 4, 4 ),
 ( 0.000000000000000000, 1.000000000000000000 ),
 .UNSPECIFIED. ) ;
#22358 = DIRECTION ( 'NONE',  ( 0.000000000000000000, 1.000000000000000000, -1.224646799147353207E-16 ) ) ;
#22359 = AXIS2_PLACEMENT_3D ( 'NONE', #9206, #303, #1937 ) ;
#22360 = CARTESIAN_POINT ( 'NONE',  ( 9.987313202862001305, -3579.494999999999891, 2239.391000000000076 ) ) ;
#22361 = EDGE_LOOP ( 'NONE', ( #2081, #12941 ) ) ;
#22362 = DIRECTION ( 'NONE',  ( 0.000000000000000000, 0.000000000000000000, -1.000000000000000000 ) ) ;
#22363 = CARTESIAN_POINT ( 'NONE',  ( 15.42885205981449737, -3543.580319130768657, 2255.300839617613747 ) ) ;
#22364 = VERTEX_POINT ( 'NONE', #14872 ) ;
#22365 = VERTEX_POINT ( 'NONE', #18828 ) ;
#22366 = ORIENTED_EDGE ( 'NONE', *, *, #11567, .F. ) ;
#22367 = DIRECTION ( 'NONE',  ( 0.000000000000000000, -1.000000000000000000, 0.000000000000000000 ) ) ;
#22368 = ORIENTED_EDGE ( 'NONE', *, *, #3971, .T. ) ;
#22369 = CIRCLE ( 'NONE', #5561, 6.476999999999001112 ) ;
#22370 = DIRECTION ( 'NONE',  ( 1.224646799147353207E-16, 1.000000000000000000, -0.000000000000000000 ) ) ;
#22371 = CARTESIAN_POINT ( 'NONE',  ( 10.81400611534258083, -3577.363169334261784, 2249.812237833679774 ) ) ;
#22372 = DIRECTION ( 'NONE',  ( 1.000000000000000000, 0.000000000000000000, 0.000000000000000000 ) ) ;
#22373 = CARTESIAN_POINT ( 'NONE',  ( 141.5988453809077896, -3581.613352772223152, 2248.107586786265529 ) ) ;
#22374 = ORIENTED_EDGE ( 'NONE', *, *, #3256, .F. ) ;
#22375 = DIRECTION ( 'NONE',  ( 1.000000000000000000, 0.000000000000000000, 0.000000000000000000 ) ) ;
#22376 = CALENDAR_DATE ( 2026, 26, 10 ) ;
#22377 = PRODUCT_RELATED_PRODUCT_CATEGORY ( 'detail', '', ( #5080 ) ) ;
#22378 = LINE ( 'NONE', #18873, #5158 ) ;
#22379 = CARTESIAN_POINT ( 'NONE',  ( 29.00679999999900005, -3568.700000000000273, 2239.009999999999764 ) ) ;
#22380 = CARTESIAN_POINT ( 'NONE',  ( 134.3871257472000025, -3657.399152860999493, 2246.630000000000109 ) ) ;
#22381 = ADVANCED_FACE ( 'NONE', ( #4427, #22113 ), #11453, .F. ) ;
#22382 = ADVANCED_FACE ( 'NONE', ( #20254 ), #9916, .F. ) ;
#22383 = ORIENTED_EDGE ( 'NONE', *, *, #14313, .F. ) ;
#22384 = CYLINDRICAL_SURFACE ( 'NONE', #2458, 1.269999999999882334 ) ;
#22385 = EDGE_CURVE ( 'NONE', #12207, #20359, #11537, .T. ) ;
#22386 = VERTEX_POINT ( 'NONE', #7596 ) ;
#22387 = CIRCLE ( 'NONE', #18290, 6.349999999999855760 ) ;
#22388 = ORIENTED_EDGE ( 'NONE', *, *, #11023, .T. ) ;
#22389 = CARTESIAN_POINT ( 'NONE',  ( 12.69999999999999929, -3583.940000000000055, 2275.055139999999483 ) ) ;
#22390 = ORIENTED_EDGE ( 'NONE', *, *, #22331, .F. ) ;
#22391 = EDGE_CURVE ( 'NONE', #8227, #11037, #20520, .T. ) ;
#22392 = CARTESIAN_POINT ( 'NONE',  ( 12.69999999999999929, -3585.210000000000036, 2268.705139999999574 ) ) ;
#22393 = DIRECTION ( 'NONE',  ( -1.000000000000000000, 0.000000000000000000, 0.000000000000000000 ) ) ;
#22394 = ORIENTED_EDGE ( 'NONE', *, *, #13504, .T. ) ;
#22395 = CARTESIAN_POINT ( 'NONE',  ( 6.988638255462328530, -3659.275913659694197, 2244.678801586293503 ) ) ;
#22396 = DIRECTION ( 'NONE',  ( -1.224646799147353207E-16, 1.000000000000000000, 0.000000000000000000 ) ) ;
#22397 = EDGE_CURVE ( 'NONE', #20612, #5300, #1835, .T. ) ;
#22398 = APPLICATION_PROTOCOL_DEFINITION ( 'international standard', 'automotive_design', 2000, #7664 ) ;
#22399 = B_SPLINE_CURVE_WITH_KNOTS ( 'NONE', 3,
 ( #13751, #1546, #10219, #15849, #17711, #21247 ),
 .UNSPECIFIED., .F., .F.,
 ( 4, 1, 1, 4 ),
 ( 0.000000000000000000, 0.3333333333333000081, 0.6666666666667000474, 1.000000000000000000 ),
 .UNSPECIFIED. ) ;
#22400 = DIRECTION ( 'NONE',  ( 0.000000000000000000, -1.000000000000000000, 0.000000000000000000 ) ) ;
#22401 = CARTESIAN_POINT ( 'NONE',  ( 12.69999999999999929, -3599.497499999999945, 2264.841800000000148 ) ) ;
#22402 = DIRECTION ( 'NONE',  ( 1.000000000000000000, 0.000000000000000000, 3.996303350731721563E-14 ) ) ;
#22403 = CIRCLE ( 'NONE', #21673, 0.7619999999999294005 ) ;
#22404 = CARTESIAN_POINT ( 'NONE',  ( 142.5447969220999767, -3659.505006299999877, 2250.165025787000104 ) ) ;
#22405 = LINE ( 'NONE', #15051, #16754 ) ;
#22406 = ORIENTED_EDGE ( 'NONE', *, *, #3964, .F. ) ;
#22407 = DIRECTION ( 'NONE',  ( -1.000000000000000000, 0.000000000000000000, 0.000000000000000000 ) ) ;
#22408 = EDGE_CURVE ( 'NONE', #19095, #16994, #13561, .T. ) ;
#22409 = VERTEX_POINT ( 'NONE', #21064 ) ;
#22410 = EDGE_LOOP ( 'NONE', ( #100, #9366, #10399, #18072 ) ) ;
#22411 = LINE ( 'NONE', #15510, #5418 ) ;
#22412 = VECTOR ( 'NONE', #6176, 1000.000000000000000 ) ;
#22413 = ADVANCED_FACE ( 'NONE', ( #15673 ), #5130, .F. ) ;
#22414 = EDGE_CURVE ( 'NONE', #17406, #22190, #22797, .T. ) ;
#22415 = CARTESIAN_POINT ( 'NONE',  ( 151.1299999999999955, -3578.860000000000127, 2247.392000000000280 ) ) ;
#22416 = EDGE_LOOP ( 'NONE', ( #14598, #4629, #15329, #16043 ) ) ;
#22417 = ORIENTED_EDGE ( 'NONE', *, *, #5225, .F. ) ;
#22418 = CARTESIAN_POINT ( 'NONE',  ( 15.54479972196000048, -3579.494985918000111, 2257.962943248000101 ) ) ;
#22419 = CARTESIAN_POINT ( 'NONE',  ( 12.70000000002484875, -3582.187400000083926, 2239.391000000000076 ) ) ;
#22420 = AXIS2_PLACEMENT_3D ( 'NONE', #16786, #629, #20422 ) ;
#22421 = DIRECTION ( 'NONE',  ( 0.7071067811865703323, 0.000000000000000000, 0.7071067811865248132 ) ) ;
#22422 = CARTESIAN_POINT ( 'NONE',  ( 25.39999999999999858, -3568.700000000000273, 2260.600000000000364 ) ) ;
#22423 = CARTESIAN_POINT ( 'NONE',  ( 12.69999999999999929, -3639.502500000000055, 2263.571799999999712 ) ) ;
#22424 = CARTESIAN_POINT ( 'NONE',  ( 15.18950216430096667, -3598.060185255141732, 2296.591799999885097 ) ) ;
#22425 = ORIENTED_EDGE ( 'NONE', *, *, #20548, .F. ) ;
#22426 = APPLICATION_PROTOCOL_DEFINITION ( 'international standard', 'automotive_design', 2000, #15302 ) ;
#22427 = ORIENTED_EDGE ( 'NONE', *, *, #9513, .T. ) ;
#22428 = LINE ( 'NONE', #11774, #20274 ) ;
#22429 = EDGE_CURVE ( 'NONE', #12173, #2094, #7146, .T. ) ;
#22430 = AXIS2_PLACEMENT_3D ( 'NONE', #16170, #18042, #21676 ) ;
#22431 = CARTESIAN_POINT ( 'NONE',  ( 57.14999999999999858, -3695.699999999999818, 2243.277199999999993 ) ) ;
#22432 = DIRECTION ( 'NONE',  ( 0.000000000000000000, 0.000000000000000000, -1.000000000000000000 ) ) ;
#22433 = APPROVAL_PERSON_ORGANIZATION ( #17109, #2891, #12069 ) ;
#22434 = ORIENTED_EDGE ( 'NONE', *, *, #10154, .F. ) ;
#22435 = DIRECTION ( 'NONE',  ( 1.000000000000000000, 0.000000000000000000, 0.000000000000000000 ) ) ;
#22436 = DIRECTION ( 'NONE',  ( 0.000000000000000000, 0.000000000000000000, -1.000000000000000000 ) ) ;
#22437 = CARTESIAN_POINT ( 'NONE',  ( 144.5596709333768786, -3662.512440222478745, 2245.822145638152051 ) ) ;
#22438 = ORIENTED_EDGE ( 'NONE', *, *, #3375, .T. ) ;
#22439 = CARTESIAN_POINT ( 'NONE',  ( 15.54479999999999862, -3579.494999999999891, 2256.063560000000052 ) ) ;
#22440 = CARTESIAN_POINT ( 'NONE',  ( 14.00164913856103155, -3662.034655424634366, 2249.514152627225485 ) ) ;
#22441 = EDGE_CURVE ( 'NONE', #20566, #14108, #22776, .T. ) ;
#22442 = EDGE_CURVE ( 'NONE', #19682, #21716, #1367, .T. ) ;
#22443 = DIRECTION ( 'NONE',  ( 2.216404975962025766E-13, 0.5000000000042060799, 0.8660254037820102058 ) ) ;
#22444 = ORIENTED_EDGE ( 'NONE', *, *, #11096, .T. ) ;
#22445 = ADVANCED_FACE ( 'NONE', ( #15786 ), #5582, .T. ) ;
#22446 = DIRECTION ( 'NONE',  ( 0.000000000000000000, 0.000000000000000000, -1.000000000000000000 ) ) ;
#22447 = CARTESIAN_POINT ( 'NONE',  ( 151.4000000000000057, 0.000000000000000000, 0.000000000000000000 ) ) ;
#22448 = CARTESIAN_POINT ( 'NONE',  ( 10.78723565514999905, -3581.600816721000228, 2246.630000000000109 ) ) ;
#22449 = CARTESIAN_POINT ( 'NONE',  ( 12.59468037889999970, -3596.652701232999789, 2279.817639764999967 ) ) ;
#22450 = DIRECTION ( 'NONE',  ( 0.000000000000000000, 0.000000000000000000, -1.000000000000000000 ) ) ;
#22451 = APPROVAL_PERSON_ORGANIZATION ( #15105, #4322, #13570 ) ;
#22452 = ORIENTED_EDGE ( 'NONE', *, *, #1080, .T. ) ;
#22453 = EDGE_CURVE ( 'NONE', #5087, #2777, #5009, .T. ) ;
#22454 = APPROVAL_PERSON_ORGANIZATION ( #18926, #20655, #8386 ) ;
#22455 = VERTEX_POINT ( 'NONE', #12150 ) ;
#22456 = AXIS2_PLACEMENT_3D ( 'NONE', #17941, #21471, #17834 ) ;
#22457 = CARTESIAN_POINT ( 'NONE',  ( 28.24479999999899604, -3670.300000000000182, 2261.869999999999891 ) ) ;
#22458 = EDGE_LOOP ( 'NONE', ( #14579, #22227, #11679, #15410, #23141 ) ) ;
#22459 = CARTESIAN_POINT ( 'NONE',  ( 15.42948858069999929, -3580.312618740999824, 2257.932964559000084 ) ) ;
#22460 = PERSON_AND_ORGANIZATION ( #16879, #19851 ) ;
#22461 = EDGE_CURVE ( 'NONE', #18833, #5647, #1439, .T. ) ;
#22462 = DIRECTION ( 'NONE',  ( -1.000000000000000000, 0.000000000000000000, 0.000000000000000000 ) ) ;
#22463 = EDGE_CURVE ( 'NONE', #4345, #6749, #18343, .T. ) ;
#22464 = DIRECTION ( 'NONE',  ( -0.000000000000000000, -1.000000000000000000, -0.000000000000000000 ) ) ;
#22465 = CARTESIAN_POINT ( 'NONE',  ( 88.90000000000000568, -3644.899999999999636, 2259.837999999999738 ) ) ;
#22466 = B_SPLINE_CURVE_WITH_KNOTS ( 'NONE', 3,
 ( #2910, #3258, #6676, #10049, #10285, #13925, #5144, #4898, #17196, #19431, #17428, #1490, #13577, #8305, #17312, #15449, #1382, #14043, #1258 ),
 .UNSPECIFIED., .F., .F.,
 ( 4, 1, 1, 1, 1, 1, 1, 1, 1, 1, 1, 1, 1, 1, 1, 1, 4 ),
 ( 3.168591426078622932E-06, 0.06250000000000000000, 0.1250000000000000000, 0.1875000000000000000, 0.2500000000000000000, 0.3125000000000000000, 0.3750000000000000000, 0.4375000000000000000, 0.5000000000000000000, 0.5625000000000000000, 0.6250000000000000000, 0.6875000000000000000, 0.7500000000000000000, 0.8125000000000000000, 0.8750000000000000000, 0.9375000000000000000, 1.000000000000000000 ),
 .UNSPECIFIED. ) ;
#22467 = FACE_OUTER_BOUND ( 'NONE', #4252, .T. ) ;
#22468 = CARTESIAN_POINT ( 'NONE',  ( 15.54479972196000048, -3659.504985917999875, 2257.962943248000101 ) ) ;
#22469 = APPLICATION_CONTEXT ( 'configuration controlled 3d designs of mechanical parts and assemblies' ) ;
#22470 = APPLIED_SECURITY_CLASSIFICATION_ASSIGNMENT ( #9398, ( #23175 ) ) ;
#22471 = VERTEX_POINT ( 'NONE', #10392 ) ;
#22472 = LOCAL_TIME ( 17, 37, 43.00000000000000000, #7656 ) ;
#22473 = CARTESIAN_POINT ( 'NONE',  ( 111.4552000000009997, -3594.099999999999909, 2259.837999999999738 ) ) ;
#22474 = DIRECTION ( 'NONE',  ( 0.000000000000000000, 0.000000000000000000, 1.000000000000000000 ) ) ;
#22475 = ORIENTED_EDGE ( 'NONE', *, *, #5999, .F. ) ;
#22476 = DIRECTION ( 'NONE',  ( 0.8660254037815640071, 0.5000000000049790172, 0.000000000000000000 ) ) ;
#22477 = CARTESIAN_POINT ( 'NONE',  ( 10.58079812952956544, -3657.607136393252858, 2248.687184364275254 ) ) ;
#22478 = VERTEX_POINT ( 'NONE', #13678 ) ;
#22479 = VECTOR ( 'NONE', #4618, 1000.000000000000000 ) ;
#22480 = ORIENTED_EDGE ( 'NONE', *, *, #16938, .T. ) ;
#22481 = VERTEX_POINT ( 'NONE', #14032 ) ;
#22482 = CARTESIAN_POINT ( 'NONE',  ( 3.048000000000000043, -3694.938000000000102, 2229.612000000000080 ) ) ;
#22483 = ORIENTED_EDGE ( 'NONE', *, *, #1679, .T. ) ;
#22484 = DIRECTION ( 'NONE',  ( 0.000000000000000000, 0.000000000000000000, -1.000000000000000000 ) ) ;
#22485 = FACE_OUTER_BOUND ( 'NONE', #20502, .T. ) ;
#22486 =( LENGTH_UNIT ( ) NAMED_UNIT ( * ) SI_UNIT ( .MILLI., .METRE. ) );
#22487 = CARTESIAN_POINT ( 'NONE',  ( 141.9350057454958574, -3581.255064581549959, 2248.927129471270291 ) ) ;
#22488 = ORIENTED_EDGE ( 'NONE', *, *, #9106, .T. ) ;
#22489 = CARTESIAN_POINT ( 'NONE',  ( 137.5573136500408395, -3581.375388660315821, 2257.800363157316951 ) ) ;
#22490 =( BOUNDED_CURVE ( )  B_SPLINE_CURVE ( 3, ( #19831, #7073, #12451, #5309 ),
 .UNSPECIFIED., .F., .F. ) 
 B_SPLINE_CURVE_WITH_KNOTS ( ( 4, 4 ),
 ( 3.686081134657729747E-14, 1.570796326492095440 ),
 .UNSPECIFIED. ) 
 CURVE ( )  GEOMETRIC_REPRESENTATION_ITEM ( )  RATIONAL_B_SPLINE_CURVE ( ( 1.000000000000000000, 0.8047378541957446174, 0.8047378541957446174, 1.000000000000000000 ) ) 
 REPRESENTATION_ITEM ( '' )  );
#22491 = PERSON_AND_ORGANIZATION ( #5446, #1895 ) ;
#22492 = DIRECTION ( 'NONE',  ( -1.000000000000000000, 0.000000000000000000, 0.000000000000000000 ) ) ;
#22493 = LINE ( 'NONE', #15363, #21225 ) ;
#22494 = CIRCLE ( 'NONE', #11630, 0.7619999999999294005 ) ;
#22495 = CARTESIAN_POINT ( 'NONE',  ( 137.3683132029000262, -3580.841199999999844, 2242.820000000000164 ) ) ;
#22496 = AXIS2_PLACEMENT_3D ( 'NONE', #11859, #17587, #22855 ) ;
#22497 = ORIENTED_EDGE ( 'NONE', *, *, #2483, .F. ) ;
#22498 = DIRECTION ( 'NONE',  ( 0.000000000000000000, -1.000000000000000000, 0.000000000000000000 ) ) ;
#22499 =( REPRESENTATION_RELATIONSHIP ('NONE','NONE', #20448, #3816 ) REPRESENTATION_RELATIONSHIP_WITH_TRANSFORMATION ( #4782 )SHAPE_REPRESENTATION_RELATIONSHIP( ) );
#22500 = ORIENTED_EDGE ( 'NONE', *, *, #2351, .F. ) ;
#22501 = CARTESIAN_POINT ( 'NONE',  ( 12.69999999997359019, -3636.810099999929662, 2296.210799999999836 ) ) ;
#22502 = APPROVAL ( #8129, 'UNSPECIFIED' ) ;
#22503 = PLANE ( 'NONE',  #11043 ) ;
#22504 = EDGE_CURVE ( 'NONE', #19328, #15238, #330, .T. ) ;
#22505 = ORIENTED_EDGE ( 'NONE', *, *, #3490, .F. ) ;
#22506 = DIRECTION ( 'NONE',  ( 0.000000000000000000, 0.000000000000000000, -1.000000000000000000 ) ) ;
#22507 = CARTESIAN_POINT ( 'NONE',  ( 139.6999999999999886, -3659.504999999999654, 2244.978999999999814 ) ) ;
#22508 = VECTOR ( 'NONE', #13626, 1000.000000000000000 ) ;
#22509 = ORIENTED_EDGE ( 'NONE', *, *, #11516, .F. ) ;
#22510 = CIRCLE ( 'NONE', #15420, 2.844800000000091700 ) ;
#22511 = DIRECTION ( 'NONE',  ( 0.000000000000000000, 0.000000000000000000, -1.000000000000000000 ) ) ;
#22512 = ADVANCED_FACE ( 'NONE', ( #4648 ), #12273, .T. ) ;
#22513 = DIRECTION ( 'NONE',  ( -2.336881798971000105E-14, 0.000000000000000000, -1.000000000000000000 ) ) ;
#22514 = EDGE_CURVE ( 'NONE', #7880, #11168, #13432, .T. ) ;
#22515 = DIRECTION ( 'NONE',  ( 1.000000000000000000, 0.000000000000000000, 0.000000000000000000 ) ) ;
#22516 = COORDINATED_UNIVERSAL_TIME_OFFSET ( 0, 0, .AHEAD. ) ;
#22517 = EDGE_CURVE ( 'NONE', #8026, #12415, #1826, .T. ) ;
#22518 = CARTESIAN_POINT ( 'NONE',  ( 20.32000000000000028, -3568.700000000000273, 2292.057900000000245 ) ) ;
#22519 = LINE ( 'NONE', #20900, #1182 ) ;
#22520 = DIRECTION ( 'NONE',  ( 0.000000000000000000, 2.336881798971000105E-14, -1.000000000000000000 ) ) ;
#22521 = DIRECTION ( 'NONE',  ( -1.000000000000000000, 0.000000000000000000, 0.000000000000000000 ) ) ;
#22522 = DIRECTION ( 'NONE',  ( -2.324635735433000053E-14, 2.336881798971000105E-14, -1.000000000000000000 ) ) ;
#22523 = ADVANCED_FACE ( 'NONE', ( #8407 ), #7094, .T. ) ;
#22524 = AXIS2_PLACEMENT_3D ( 'NONE', #19016, #21127, #12215 ) ;
#22525 = ORIENTED_EDGE ( 'NONE', *, *, #10137, .F. ) ;
#22526 = CIRCLE ( 'NONE', #18426, 2.844800000000091700 ) ;
#22527 = CARTESIAN_POINT ( 'NONE',  ( 76.20000000000000284, -3670.300000000000182, 2239.771999999999935 ) ) ;
#22528 = CIRCLE ( 'NONE', #19186, 0.7619999999999294005 ) ;
#22529 = ORIENTED_EDGE ( 'NONE', *, *, #18147, .F. ) ;
#22530 = FACE_OUTER_BOUND ( 'NONE', #772, .T. ) ;
#22531 = FACE_OUTER_BOUND ( 'NONE', #10852, .T. ) ;
#22532 = VERTEX_POINT ( 'NONE', #15554 ) ;
#22533 = EDGE_LOOP ( 'NONE', ( #5822, #48, #6569, #2104 ) ) ;
#22534 = DIRECTION ( 'NONE',  ( -1.000000000000000000, 0.000000000000000000, 0.000000000000000000 ) ) ;
#22535 = CARTESIAN_POINT ( 'NONE',  ( 17.78000000000000114, -3659.504999999999654, 2244.978999999999814 ) ) ;
#22536 = VECTOR ( 'NONE', #20326, 1000.000000000000000 ) ;
#22537 = CARTESIAN_POINT ( 'NONE',  ( 12.07314413848000001, -3602.278404630999830, 2279.801389126999766 ) ) ;
#22538 = EDGE_LOOP ( 'NONE', ( #10028, #22505, #18485, #4757 ) ) ;
#22539 = EDGE_CURVE ( 'NONE', #7881, #13900, #18667, .T. ) ;
#22540 = FACE_OUTER_BOUND ( 'NONE', #5436, .T. ) ;
#22541 = DIRECTION ( 'NONE',  ( -3.308571459023000057E-13, 2.590196616237999979E-13, -1.000000000000000000 ) ) ;
#22542 = EDGE_CURVE ( 'NONE', #20662, #11168, #82, .T. ) ;
#22543 = CARTESIAN_POINT ( 'NONE',  ( 139.6999999999999886, -3656.660200000000714, 2257.592639999999847 ) ) ;
#22544 = AXIS2_PLACEMENT_3D ( 'NONE', #6314, #8289, #21922 ) ;
#22545 = CARTESIAN_POINT ( 'NONE',  ( 20.66649961935109303, -3695.634659422622462, 2259.732127985863372 ) ) ;
#22546 = EDGE_CURVE ( 'NONE', #5890, #2680, #17768, .T. ) ;
#22547 = EDGE_LOOP ( 'NONE', ( #10592, #9042, #9185, #18251 ) ) ;
#22548 = PERSON_AND_ORGANIZATION_ROLE ( 'design_supplier' ) ;
#22549 = ADVANCED_FACE ( 'NONE', ( #8983 ), #11199, .T. ) ;
#22550 = CIRCLE ( 'NONE', #16928, 5.715000000000997282 ) ;
#22551 = VERTEX_POINT ( 'NONE', #2075 ) ;
#22552 = CARTESIAN_POINT ( 'NONE',  ( 10.21049783553828050, -3638.065185255057713, 2296.591800000037438 ) ) ;
#22553 = CIRCLE ( 'NONE', #5366, 2.844800000000091700 ) ;
#22554 = CARTESIAN_POINT ( 'NONE',  ( 10.90907282900277409, -3581.705358305645859, 2247.446708594144638 ) ) ;
#22555 = DIRECTION ( 'NONE',  ( 0.000000000000000000, 0.000000000000000000, 1.000000000000000000 ) ) ;
#22556 = VERTEX_POINT ( 'NONE', #14613 ) ;
#22557 = CIRCLE ( 'NONE', #18813, 2.844800000000091700 ) ;
#22558 = DIRECTION ( 'NONE',  ( 0.000000000000000000, 0.000000000000000000, -1.000000000000000000 ) ) ;
#22559 = EDGE_CURVE ( 'NONE', #15832, #7984, #13865, .T. ) ;
#22560 = CARTESIAN_POINT ( 'NONE',  ( 50.79999999999999716, -3670.300000000000182, 2259.837999999999738 ) ) ;
#22561 = CARTESIAN_POINT ( 'NONE',  ( 144.6090632468122976, -3662.431858318084778, 2245.704773982281495 ) ) ;
#22562 = CIRCLE ( 'NONE', #19217, 0.7619999999999294005 ) ;
#22563 = DIRECTION ( 'NONE',  ( 0.000000000000000000, 0.000000000000000000, 1.000000000000000000 ) ) ;
#22564 = CARTESIAN_POINT ( 'NONE',  ( 11.95719394751944620, -3662.251176165646939, 2249.298813514415542 ) ) ;
#22565 = CIRCLE ( 'NONE', #504, 0.7620000000000000107 ) ;
#22566 = CARTESIAN_POINT ( 'NONE',  ( -5.588000000000000078, -3578.860000000000127, 2244.547199999999975 ) ) ;
#22567 = ORIENTED_EDGE ( 'NONE', *, *, #20232, .T. ) ;
#22568 = CARTESIAN_POINT ( 'NONE',  ( 127.0000000000000000, -3619.500000000000000, 2259.837999999999738 ) ) ;
#22569 = CARTESIAN_POINT ( 'NONE',  ( 9.987313202835000681, -3597.931329546999677, 2296.591799999999694 ) ) ;
#22570 = CARTESIAN_POINT ( 'NONE',  ( 88.90000000000000568, -3594.099999999999909, 2261.869999999999891 ) ) ;
#22571 = DIRECTION ( 'NONE',  ( 0.000000000000000000, 0.000000000000000000, -1.000000000000000000 ) ) ;
#22572 = PLANE ( 'NONE',  #10955 ) ;
#22573 = AXIS2_PLACEMENT_3D ( 'NONE', #22423, #6396, #10018 ) ;
#22574 = ORIENTED_EDGE ( 'NONE', *, *, #7383, .F. ) ;
#22575 = CARTESIAN_POINT ( 'NONE',  ( 116.8400000000000034, -3543.300000000000182, 2243.277199999999993 ) ) ;
#22576 = EDGE_LOOP ( 'NONE', ( #16550, #19938, #3924, #11302 ) ) ;
#22577 = CARTESIAN_POINT ( 'NONE',  ( 141.1353819475458522, -3657.021135561388746, 2257.680384087519542 ) ) ;
#22578 = APPROVAL_STATUS ( 'not_yet_approved' ) ;
#22579 = EDGE_CURVE ( 'NONE', #6658, #15033, #10506, .T. ) ;
#22580 = DIRECTION ( 'NONE',  ( 1.000000000000000000, 0.000000000000000000, 3.996303350731721563E-14 ) ) ;
#22581 = EDGE_CURVE ( 'NONE', #4464, #18295, #20189, .T. ) ;
#22582 = CARTESIAN_POINT ( 'NONE',  ( 147.8270794805000037, -3543.299999999999727, 2259.329999999999927 ) ) ;
#22583 = DIRECTION ( 'NONE',  ( 0.000000000000000000, 0.000000000000000000, -1.000000000000000000 ) ) ;
#22584 = CARTESIAN_POINT ( 'NONE',  ( 13.78135004281000064, -3656.868789907000064, 2257.644359223000265 ) ) ;
#22585 = CARTESIAN_POINT ( 'NONE',  ( 10.78733304872000076, -3657.399152860999493, 2246.630000000000109 ) ) ;
#22586 = FACE_OUTER_BOUND ( 'NONE', #3203, .T. ) ;
#22587 = EDGE_CURVE ( 'NONE', #3605, #4945, #3328, .T. ) ;
#22588 = VERTEX_POINT ( 'NONE', #10856 ) ;
#22589 = AXIS2_PLACEMENT_3D ( 'NONE', #14175, #15802, #8892 ) ;
#22590 = CARTESIAN_POINT ( 'NONE',  ( 101.5999999999999943, -3670.300000000000182, 2259.837999999999738 ) ) ;
#22591 = LINE ( 'NONE', #801, #8807 ) ;
#22592 = ORIENTED_EDGE ( 'NONE', *, *, #11641, .F. ) ;
#22593 = CARTESIAN_POINT ( 'NONE',  ( 10.55978476029679491, -3657.630734846978157, 2248.732827181204811 ) ) ;
#22594 = ADVANCED_FACE ( 'NONE', ( #18004 ), #9108, .F. ) ;
#22595 = ORIENTED_EDGE ( 'NONE', *, *, #10723, .F. ) ;
#22596 = EDGE_CURVE ( 'NONE', #14057, #15010, #22403, .T. ) ;
#22597 = VERTEX_POINT ( 'NONE', #14501 ) ;
#22598 = CARTESIAN_POINT ( 'NONE',  ( 142.0316867971999955, -3660.851200000000063, 2239.391000000000076 ) ) ;
#22599 = EDGE_LOOP ( 'NONE', ( #14037, #21549, #6683, #18359 ) ) ;
#22600 = DIRECTION ( 'NONE',  ( 0.000000000000000000, 1.000000000000000000, 0.000000000000000000 ) ) ;
#22601 = CARTESIAN_POINT ( 'NONE',  ( 105.2067999999999870, -3568.700000000000273, 2260.600000000000364 ) ) ;
#22602 = DIRECTION ( 'NONE',  ( 1.000000000000000000, 0.000000000000000000, 0.000000000000000000 ) ) ;
#22603 = DIRECTION ( 'NONE',  ( 0.6887494619146554697, 0.000000000000000000, -0.7249994335944496271 ) ) ;
#22604 = ORIENTED_EDGE ( 'NONE', *, *, #16524, .T. ) ;
#22605 = CARTESIAN_POINT ( 'NONE',  ( 131.8996122109008979, -3695.401597382865475, 2260.148187843663891 ) ) ;
#22606 = CIRCLE ( 'NONE', #8033, 6.349999999999855760 ) ;
#22607 = PRODUCT_CONTEXT ( 'NONE', #22469, 'mechanical' ) ;
#22608 = AXIS2_PLACEMENT_3D ( 'NONE', #9880, #8143, #15286 ) ;
#22609 = EDGE_CURVE ( 'NONE', #10895, #21188, #21299, .T. ) ;
#22610 = TOROIDAL_SURFACE ( 'NONE', #11376, 3.606799999999999784, 0.7620000000000000107 ) ;
#22611 = CARTESIAN_POINT ( 'NONE',  ( 10.36831320283000046, -3600.843699999999899, 2296.210799999999836 ) ) ;
#22612 = DIRECTION ( 'NONE',  ( 0.000000000000000000, 0.000000000000000000, 1.000000000000000000 ) ) ;
#22613 = CARTESIAN_POINT ( 'NONE',  ( 127.0000000000000000, -3578.860000000000127, 2247.392000000000280 ) ) ;
#22614 = VERTEX_POINT ( 'NONE', #5712 ) ;
#22615 = CARTESIAN_POINT ( 'NONE',  ( 12.69999999999999929, -3576.320000000000164, 2245.359999999999673 ) ) ;
#22616 = CARTESIAN_POINT ( 'NONE',  ( 20.32000000000000028, -3544.061999999999898, 2292.057900000000245 ) ) ;
#22617 = VERTEX_POINT ( 'NONE', #20004 ) ;
#22618 = TOROIDAL_SURFACE ( 'NONE', #6611, 5.080000000000000071, 0.3810000000000000053 ) ;
#22619 = DIRECTION ( 'NONE',  ( 0.000000000000000000, 0.000000000000000000, -1.000000000000000000 ) ) ;
#22620 = TOROIDAL_SURFACE ( 'NONE', #8049, 4.114799999999999791, 1.270000000000000018 ) ;
#22621 = VECTOR ( 'NONE', #17674, 1000.000000000000000 ) ;
#22622 = FACE_OUTER_BOUND ( 'NONE', #21376, .T. ) ;
#22623 = AXIS2_PLACEMENT_3D ( 'NONE', #12353, #20788, #10474 ) ;
#22624 = ORIENTED_EDGE ( 'NONE', *, *, #9302, .F. ) ;
#22625 = VERTEX_POINT ( 'NONE', #23145 ) ;
#22626 = CARTESIAN_POINT ( 'NONE',  ( 139.6999999999986528, -3582.187400000179423, 2239.167815367220555 ) ) ;
#22627 = SPHERICAL_SURFACE ( 'NONE', #13281, 0.7620000000000000107 ) ;
#22628 = ORIENTED_EDGE ( 'NONE', *, *, #20614, .T. ) ;
#22629 = CARTESIAN_POINT ( 'NONE',  ( 3.810000000000000053, -3544.061999999999898, 2238.248000000000047 ) ) ;
#22630 = CARTESIAN_POINT ( 'NONE',  ( 136.8552000000009912, -3659.504999999999654, 2272.030000000000200 ) ) ;
#22631 = DIRECTION ( 'NONE',  ( -1.000000000000000000, 0.000000000000000000, 0.000000000000000000 ) ) ;
#22632 = DIRECTION ( 'NONE',  ( -1.000000000000000000, 0.000000000000000000, 0.000000000000000000 ) ) ;
#22633 = DATE_AND_TIME ( #15738, #19072 ) ;
#22634 = LINE ( 'NONE', #3189, #953 ) ;
#22635 = LINE ( 'NONE', #6376, #21780 ) ;
#22636 = CARTESIAN_POINT ( 'NONE',  ( 18.41499991942999870, -3579.495498070999474, 2244.618783703000190 ) ) ;
#22637 = CIRCLE ( 'NONE', #6197, 1.269999999999882334 ) ;
#22638 = AXIS2_PLACEMENT_3D ( 'NONE', #18625, #10058, #916 ) ;
#22639 = PRODUCT_DEFINITION ( 'UNKNOWN', '', #741, #2927 ) ;
#22640 = AXIS2_PLACEMENT_3D ( 'NONE', #21553, #2213, #3724 ) ;
#22641 = CARTESIAN_POINT ( 'NONE',  ( 142.0593047748026265, -3657.915120415264937, 2249.165646973382536 ) ) ;
#22642 = CIRCLE ( 'NONE', #14050, 5.460999999999938126 ) ;
#22643 = ORIENTED_EDGE ( 'NONE', *, *, #2760, .T. ) ;
#22644 = CIRCLE ( 'NONE', #9932, 0.7619999999999294005 ) ;
#22645 = CARTESIAN_POINT ( 'NONE',  ( 12.69999999999999929, -3579.494999999999891, 2272.030000000000200 ) ) ;
#22646 = ADVANCED_FACE ( 'NONE', ( #19776 ), #17647, .T. ) ;
#22647 = ORIENTED_EDGE ( 'NONE', *, *, #79, .F. ) ;
#22648 = CARTESIAN_POINT ( 'NONE',  ( 4.572920519510999426, -3695.699999999999818, 2259.329999999999927 ) ) ;
#22649 = CARTESIAN_POINT ( 'NONE',  ( -8.890000000026999416, -3657.447599999999966, 2247.392000000000280 ) ) ;
#22650 = VERTEX_POINT ( 'NONE', #1597 ) ;
#22651 = EDGE_LOOP ( 'NONE', ( #16095, #9615, #22903, #3013, #7966, #11998 ) ) ;
#22652 = CARTESIAN_POINT ( 'NONE',  ( -6.730999999999999872, -3660.140000000000327, 2247.392000000000280 ) ) ;
#22653 = AXIS2_PLACEMENT_3D ( 'NONE', #11092, #7682, #16362 ) ;
#22654 = DIRECTION ( 'NONE',  ( 0.000000000000000000, 1.000000000000000000, 0.000000000000000000 ) ) ;
#22655 = AXIS2_PLACEMENT_3D ( 'NONE', #20219, #1090, #20335 ) ;
#22656 = DIRECTION ( 'NONE',  ( 1.000000000000000000, 0.000000000000000000, 0.000000000000000000 ) ) ;
#22657 = ORIENTED_EDGE ( 'NONE', *, *, #9010, .T. ) ;
#22658 = AXIS2_PLACEMENT_3D ( 'NONE', #8545, #10168, #12165 ) ;
#22659 = DIRECTION ( 'NONE',  ( 0.000000000000000000, 0.000000000000000000, -1.000000000000000000 ) ) ;
#22660 = DIRECTION ( 'NONE',  ( 0.000000000000000000, 0.000000000000000000, -1.000000000000000000 ) ) ;
#22661 = CIRCLE ( 'NONE', #6202, 5.714999999999998082 ) ;
#22662 = CARTESIAN_POINT ( 'NONE',  ( 147.3199999999999932, -3694.430000000000291, 2260.600000000000364 ) ) ;
#22663 = PLANE ( 'NONE',  #17712 ) ;
#22664 = CARTESIAN_POINT ( 'NONE',  ( 14.05634339859000015, -3577.145744321000166, 2239.391000000000076 ) ) ;
#22665 = ORIENTED_EDGE ( 'NONE', *, *, #2664, .T. ) ;
#22666 = DATE_AND_TIME ( #11768, #5264 ) ;
#22667 = ORIENTED_EDGE ( 'NONE', *, *, #20668, .F. ) ;
#22668 = CIRCLE ( 'NONE', #16328, 2.873832635400752622 ) ;
#22669 = CARTESIAN_POINT ( 'NONE',  ( 10.36831320283682167, -3638.156299999849125, 2296.433984632765714 ) ) ;
#22670 = APPLIED_PERSON_AND_ORGANIZATION_ASSIGNMENT ( #932, #9955, ( #16320 ) ) ;
#22671 = CARTESIAN_POINT ( 'NONE',  ( 10.25511876121471211, -3580.949311574155672, 2249.322936109902002 ) ) ;
#22672 = PLANE ( 'NONE',  #3711 ) ;
#22673 = CIRCLE ( 'NONE', #18932, 2.844800000000091700 ) ;
#22674 = ORIENTED_EDGE ( 'NONE', *, *, #21820, .T. ) ;
#22675 = AXIS2_PLACEMENT_3D ( 'NONE', #22415, #14946, #22189 ) ;
#22676 = DIRECTION ( 'NONE',  ( 1.000000000000000000, 0.000000000000000000, 0.000000000000000000 ) ) ;
#22677 = AXIS2_PLACEMENT_3D ( 'NONE', #21729, #7320, #12932 ) ;
#22678 = ADVANCED_FACE ( 'NONE', ( #3703 ), #1837, .T. ) ;
#22679 = EDGE_CURVE ( 'NONE', #19336, #2102, #16246, .T. ) ;
#22680 = CARTESIAN_POINT ( 'NONE',  ( 151.1299999999999955, -3694.430000000000291, 2259.329999999999927 ) ) ;
#22681 = CARTESIAN_POINT ( 'NONE',  ( 144.5842015178808708, -3662.472695314643261, 2245.762539381157694 ) ) ;
#22682 = LINE ( 'NONE', #8750, #9240 ) ;
#22683 = CARTESIAN_POINT ( 'NONE',  ( 11.14436922434143895, -3661.887241596394233, 2249.637207235594815 ) ) ;
#22684 = EDGE_CURVE ( 'NONE', #4703, #20008, #21411, .T. ) ;
#22685 = CARTESIAN_POINT ( 'NONE',  ( 15.54478140927793284, -3659.506684851170121, 2250.165409776138404 ) ) ;
#22686 = AXIS2_PLACEMENT_3D ( 'NONE', #14146, #1240, #8522 ) ;
#22687 = VERTEX_POINT ( 'NONE', #12731 ) ;
#22688 = CARTESIAN_POINT ( 'NONE',  ( -5.588000000000000078, -3544.061999999999898, 2228.849999999999909 ) ) ;
#22689 = FACE_OUTER_BOUND ( 'NONE', #13107, .T. ) ;
#22690 = CARTESIAN_POINT ( 'NONE',  ( 9.987313202864001482, -3661.071170452999922, 2239.009999999999764 ) ) ;
#22691 = CARTESIAN_POINT ( 'NONE',  ( 14.47352478144048327, -3657.280624183466898, 2247.292342066113633 ) ) ;
#22692 = DIRECTION ( 'NONE',  ( -1.000000000000000000, 0.000000000000000000, 0.000000000000000000 ) ) ;
#22693 = ORIENTED_EDGE ( 'NONE', *, *, #8014, .T. ) ;
#22694 = ORIENTED_EDGE ( 'NONE', *, *, #18857, .F. ) ;
#22695 = CIRCLE ( 'NONE', #20107, 3.606799999999993567 ) ;
#22696 = CARTESIAN_POINT ( 'NONE',  ( 142.0316867971999955, -3660.851200000000063, 2242.820000000000164 ) ) ;
#22697 = EDGE_CURVE ( 'NONE', #5364, #22614, #3715, .T. ) ;
#22698 = ORIENTED_EDGE ( 'NONE', *, *, #20969, .T. ) ;
#22699 = CIRCLE ( 'NONE', #17464, 2.844799999999009010 ) ;
#22700 = CARTESIAN_POINT ( 'NONE',  ( 139.6999999999999886, -3656.660200000000714, 2257.592639999999847 ) ) ;
#22701 = TOROIDAL_SURFACE ( 'NONE', #3618, 3.606799999999999784, 0.7620000000000000107 ) ;
#22702 = COORDINATED_UNIVERSAL_TIME_OFFSET ( 0, 0, .AHEAD. ) ;
#22703 = DIRECTION ( 'NONE',  ( 0.000000000000000000, 0.000000000000000000, 1.000000000000000000 ) ) ;
#22704 = EDGE_LOOP ( 'NONE', ( #18678, #12230, #12361, #20475 ) ) ;
#22705 = CARTESIAN_POINT ( 'NONE',  ( 72.59320000000001016, -3670.300000000000182, 2239.771999999999935 ) ) ;
#22706 = FACE_OUTER_BOUND ( 'NONE', #14923, .T. ) ;
#22707 = CARTESIAN_POINT ( 'NONE',  ( 137.1599999999999966, -3694.430000000000291, 2255.774000000000342 ) ) ;
#22708 = CARTESIAN_POINT ( 'NONE',  ( 101.5999999999999943, -3568.700000000000273, 2261.869999999999891 ) ) ;
#22709 = DIRECTION ( 'NONE',  ( 0.000000000000000000, -1.000000000000000000, 0.000000000000000000 ) ) ;
#22710 = ORIENTED_EDGE ( 'NONE', *, *, #774, .F. ) ;
#22711 = DIRECTION ( 'NONE',  ( 0.000000000000000000, -1.000000000000000000, 0.000000000000000000 ) ) ;
#22712 = EDGE_CURVE ( 'NONE', #8944, #18606, #8964, .T. ) ;
#22713 = AXIS2_PLACEMENT_3D ( 'NONE', #9022, #14191, #5522 ) ;
#22714 = LINE ( 'NONE', #19557, #22266 ) ;
#22715 = ORIENTED_EDGE ( 'NONE', *, *, #11102, .F. ) ;
#22716 = CARTESIAN_POINT ( 'NONE',  ( 20.32000000000000028, -3568.700000000000273, 2289.213099999999940 ) ) ;
#22717 = CARTESIAN_POINT ( 'NONE',  ( 10.61582386584563764, -3657.568526570700215, 2248.609309335925900 ) ) ;
#22718 = EDGE_CURVE ( 'NONE', #22455, #7086, #4090, .T. ) ;
#22719 = ORIENTED_EDGE ( 'NONE', *, *, #4003, .F. ) ;
#22720 = ADVANCED_FACE ( 'NONE', ( #18683 ), #6728, .T. ) ;
#22721 = AXIS2_PLACEMENT_3D ( 'NONE', #19228, #19107, #11843 ) ;
#22722 = ORIENTED_EDGE ( 'NONE', *, *, #8578, .F. ) ;
#22723 = DIRECTION ( 'NONE',  ( 0.000000000000000000, 0.000000000000000000, 1.000000000000000000 ) ) ;
#22724 = EDGE_LOOP ( 'NONE', ( #22270, #3200, #9843, #21319 ) ) ;
#22725 = LINE ( 'NONE', #17563, #6601 ) ;
#22726 = DIRECTION ( 'NONE',  ( -1.000000000000000000, 0.000000000000000000, 0.000000000000000000 ) ) ;
#22727 = ORIENTED_EDGE ( 'NONE', *, *, #21970, .T. ) ;
#22728 = CARTESIAN_POINT ( 'NONE',  ( 3.048000000000000043, -3694.938000000000102, 2239.009999999999764 ) ) ;
#22729 = DATE_AND_TIME ( #1407, #5625 ) ;
#22730 = AXIS2_PLACEMENT_3D ( 'NONE', #208, #17656, #7359 ) ;
#22731 = PLANE ( 'NONE',  #8145 ) ;
#22732 = DIRECTION ( 'NONE',  ( 1.678948246106317188E-14, 0.000000000000000000, -1.000000000000000000 ) ) ;
#22733 = EDGE_CURVE ( 'NONE', #11364, #982, #16433, .T. ) ;
#22734 = AXIS2_PLACEMENT_3D ( 'NONE', #13063, #2286, #5693 ) ;
#22735 = CARTESIAN_POINT ( 'NONE',  ( 134.1280881846921886, -3658.234155390725846, 2245.279838229026609 ) ) ;
#22736 = DIRECTION ( 'NONE',  ( 1.000000000000000000, 0.000000000000000000, 0.000000000000000000 ) ) ;
#22737 = ORIENTED_EDGE ( 'NONE', *, *, #11868, .T. ) ;
#22738 = CARTESIAN_POINT ( 'NONE',  ( 15.42897132338017130, -3695.419680871121727, 2255.300887234111087 ) ) ;
#22739 = CARTESIAN_POINT ( 'NONE',  ( 29.00679999999900005, -3568.700000000000273, 2260.600000000000364 ) ) ;
#22740 = ORIENTED_EDGE ( 'NONE', *, *, #1099, .F. ) ;
#22741 = DIRECTION ( 'NONE',  ( 0.000000000000000000, 0.000000000000000000, 1.000000000000000000 ) ) ;
#22742 = AXIS2_PLACEMENT_3D ( 'NONE', #7763, #2486, #9847 ) ;
#22743 = EDGE_CURVE ( 'NONE', #767, #18606, #8031, .T. ) ;
#22744 = CARTESIAN_POINT ( 'NONE',  ( 139.6999999999999886, -3661.409999999999400, 2272.030000000000200 ) ) ;
#22745 = ORIENTED_EDGE ( 'NONE', *, *, #9968, .T. ) ;
#22746 = EDGE_LOOP ( 'NONE', ( #9386, #7530, #3796, #13991 ) ) ;
#22747 = CARTESIAN_POINT ( 'NONE',  ( 139.6999999997610757, -3582.627340905411984, 2239.009999999999764 ) ) ;
#22748 = CARTESIAN_POINT ( 'NONE',  ( 133.9879525578283221, -3659.716236870563534, 2244.576910402178783 ) ) ;
#22749 = VERTEX_POINT ( 'NONE', #11311 ) ;
#22750 = DIRECTION ( 'NONE',  ( -0.000000000000000000, -0.000000000000000000, -1.000000000000000000 ) ) ;
#22751 = DIRECTION ( 'NONE',  ( 0.9296367896514280416, -0.3684771896964403326, 0.000000000000000000 ) ) ;
#22752 = LINE ( 'NONE', #1308, #1989 ) ;
#22753 = PLANE ( 'NONE',  #3613 ) ;
#22754 = COORDINATED_UNIVERSAL_TIME_OFFSET ( 0, 0, .AHEAD. ) ;
#22755 = CARTESIAN_POINT ( 'NONE',  ( 6.985153502415998972, -3659.715133692337531, 2244.570904742638959 ) ) ;
#22756 = DIRECTION ( 'NONE',  ( 0.000000000000000000, 0.000000000000000000, -1.000000000000000000 ) ) ;
#22757 = CARTESIAN_POINT ( 'NONE',  ( 18.39651424583543005, -3579.956683882389825, 2244.766317903216077 ) ) ;
#22758 = ADVANCED_FACE ( 'NONE', ( #15181 ), #12966, .T. ) ;
#22759 = EDGE_CURVE ( 'NONE', #16226, #20085, #11423, .T. ) ;
#22760 = CARTESIAN_POINT ( 'NONE',  ( 141.6278228631028355, -3657.412925642543541, 2248.202207075162733 ) ) ;
#22761 = ORIENTED_EDGE ( 'NONE', *, *, #1099, .T. ) ;
#22762 = AXIS2_PLACEMENT_3D ( 'NONE', #566, #11561, #22004 ) ;
#22763 = CARTESIAN_POINT ( 'NONE',  ( 35.56000000000000227, -3695.699999999999818, 2247.392000000000280 ) ) ;
#22764 = VERTEX_POINT ( 'NONE', #754 ) ;
#22765 = ORIENTED_EDGE ( 'NONE', *, *, #4408, .F. ) ;
#22766 = CARTESIAN_POINT ( 'NONE',  ( 139.6999999999999886, -3579.494999999999891, 2246.630000000000109 ) ) ;
#22767 = VERTEX_POINT ( 'NONE', #14953 ) ;
#22768 = ORIENTED_EDGE ( 'NONE', *, *, #12163, .F. ) ;
#22769 = CARTESIAN_POINT ( 'NONE',  ( 20.32000000000000028, -3670.300000000000182, 2292.057900000000245 ) ) ;
#22770 = CARTESIAN_POINT ( 'NONE',  ( 79.04479999999999507, -3670.300000000000182, 2259.837999999999738 ) ) ;
#22771 = DIRECTION ( 'NONE',  ( -1.000000000000000000, 0.000000000000000000, 0.000000000000000000 ) ) ;
#22772 = EDGE_LOOP ( 'NONE', ( #12051, #19965, #12341, #1867 ) ) ;
#22773 = DIRECTION ( 'NONE',  ( -0.000000000000000000, -1.000000000000000000, -0.000000000000000000 ) ) ;
#22774 = CARTESIAN_POINT ( 'NONE',  ( 9.855200508358999301, -3579.494986006000545, 2257.962940201000038 ) ) ;
#22775 = CARTESIAN_POINT ( 'NONE',  ( 131.7757523116999891, -3694.430000000000291, 2260.600000000000364 ) ) ;
#22776 = CIRCLE ( 'NONE', #9674, 0.7619999999999294005 ) ;
#22777 = FACE_OUTER_BOUND ( 'NONE', #19002, .T. ) ;
#22778 = VERTEX_POINT ( 'NONE', #14846 ) ;
#22779 = APPROVAL_STATUS ( 'not_yet_approved' ) ;
#22780 = VERTEX_POINT ( 'NONE', #13417 ) ;
#22781 = FACE_OUTER_BOUND ( 'NONE', #13942, .T. ) ;
#22782 = CARTESIAN_POINT ( 'NONE',  ( 10.48988688109928091, -3581.286862158647182, 2248.877936337259598 ) ) ;
#22783 = DIRECTION ( 'NONE',  ( -1.000000000000000000, 0.000000000000000000, 0.000000000000000000 ) ) ;
#22784 = ORIENTED_EDGE ( 'NONE', *, *, #902, .F. ) ;
#22785 = ORIENTED_EDGE ( 'NONE', *, *, #19843, .T. ) ;
#22786 = FACE_BOUND ( 'NONE', #16476, .T. ) ;
#22787 = CARTESIAN_POINT ( 'NONE',  ( 12.69999999999999929, -3648.710000000000036, 2268.705139999999574 ) ) ;
#22788 = CARTESIAN_POINT ( 'NONE',  ( 144.3368584422871379, -3662.846051980176981, 2246.504844866363328 ) ) ;
#22789 = AXIS2_PLACEMENT_3D ( 'NONE', #18232, #7915, #4167 ) ;
#22790 = CARTESIAN_POINT ( 'NONE',  ( 131.8084955422000064, -3694.472271328999796, 2260.600000000000364 ) ) ;
#22791 = CARTESIAN_POINT ( 'NONE',  ( 12.37593526700610447, -3662.332104801266269, 2249.205209426644615 ) ) ;
#22792 = CARTESIAN_POINT ( 'NONE',  ( 95.25000000000000000, -3694.430000000000291, 2244.547199999999975 ) ) ;
#22793 = VERTEX_POINT ( 'NONE', #20453 ) ;
#22794 = DIRECTION ( 'NONE',  ( 2.336881798971000105E-14, 0.000000000000000000, 1.000000000000000000 ) ) ;
#22795 = DIRECTION ( 'NONE',  ( 0.000000000000000000, -1.000000000000000000, 0.000000000000000000 ) ) ;
#22796 = PRODUCT_DEFINITION ( 'UNKNOWN', '', #2608, #10183 ) ;
#22797 = LINE ( 'NONE', #17531, #19802 ) ;
#22798 = CARTESIAN_POINT ( 'NONE',  ( 12.70000000000017693, -3582.670000000000073, 2245.359999999999673 ) ) ;
#22799 = CARTESIAN_POINT ( 'NONE',  ( -12.31899999999987827, -3576.167599999831964, 2247.391999999993914 ) ) ;
#22800 = ORIENTED_EDGE ( 'NONE', *, *, #16015, .F. ) ;
#22801 = EDGE_LOOP ( 'NONE', ( #19633, #7642, #4749, #19673, #3911, #3038, #10669, #19990 ) ) ;
#22802 = EDGE_CURVE ( 'NONE', #6791, #20799, #14951, .T. ) ;
#22803 = VERTEX_POINT ( 'NONE', #22083 ) ;
#22804 = DIRECTION ( 'NONE',  ( -1.000000000000000000, 0.000000000000000000, 0.000000000000000000 ) ) ;
#22805 = LOCAL_TIME ( 17, 37, 43.00000000000000000, #13369 ) ;
#22806 = ADVANCED_FACE ( 'NONE', ( #13300 ), #4285, .F. ) ;
#22807 = ORIENTED_EDGE ( 'NONE', *, *, #20167, .T. ) ;
#22808 = AXIS2_PLACEMENT_3D ( 'NONE', #18798, #1100, #8261 ) ;
#22809 = DIRECTION ( 'NONE',  ( 0.000000000000000000, 0.000000000000000000, -1.000000000000000000 ) ) ;
#22810 = PERSON_AND_ORGANIZATION ( #21087, #13873 ) ;
#22811 = EDGE_CURVE ( 'NONE', #19948, #17590, #19821, .T. ) ;
#22812 = DIRECTION ( 'NONE',  ( 0.000000000000000000, -1.000000000000000000, 0.000000000000000000 ) ) ;
#22813 = CARTESIAN_POINT ( 'NONE',  ( 130.6067999999989979, -3670.300000000000182, 2259.837999999999738 ) ) ;
#22814 = CARTESIAN_POINT ( 'NONE',  ( 12.69999999999999929, -3599.497499999999945, 2288.971800000000258 ) ) ;
#22815 = FACE_OUTER_BOUND ( 'NONE', #13360, .T. ) ;
#22816 = DIRECTION ( 'NONE',  ( 1.000000000000000000, 0.000000000000000000, 0.000000000000000000 ) ) ;
#22817 = EDGE_CURVE ( 'NONE', #1200, #18510, #2301, .T. ) ;
#22818 = FACE_OUTER_BOUND ( 'NONE', #19155, .T. ) ;
#22819 = ORIENTED_EDGE ( 'NONE', *, *, #22294, .F. ) ;
#22820 = CIRCLE ( 'NONE', #4133, 5.460999999999938126 ) ;
#22821 = DIRECTION ( 'NONE',  ( -1.000000000000000000, 2.318894227180000040E-14, 2.343004830739999973E-14 ) ) ;
#22822 = VERTEX_POINT ( 'NONE', #9447 ) ;
#22823 = LOCAL_TIME ( 17, 37, 43.00000000000000000, #9814 ) ;
#22824 = EDGE_CURVE ( 'NONE', #21968, #8227, #12711, .T. ) ;
#22825 = DIRECTION ( 'NONE',  ( 0.000000000000000000, 1.000000000000000000, 0.000000000000000000 ) ) ;
#22826 = CARTESIAN_POINT ( 'NONE',  ( 10.07389198931091379, -3658.410956137315225, 2249.651275816309408 ) ) ;
#22827 = ORIENTED_EDGE ( 'NONE', *, *, #14021, .T. ) ;
#22828 = CIRCLE ( 'NONE', #8626, 11.11249999999999716 ) ;
#22829 = CARTESIAN_POINT ( 'NONE',  ( 123.3932000000010021, -3568.700000000000273, 2239.009999999999764 ) ) ;
#22830 = ORIENTED_EDGE ( 'NONE', *, *, #3677, .F. ) ;
#22831 = CARTESIAN_POINT ( 'NONE',  ( 22.54063073453000143, -3543.299999999999727, 2275.763800000000174 ) ) ;
#22832 = PERSON_AND_ORGANIZATION ( #5446, #1895 ) ;
#22833 = FACE_OUTER_BOUND ( 'NONE', #14684, .T. ) ;
#22834 = EDGE_LOOP ( 'NONE', ( #252, #5508, #15169, #170 ) ) ;
#22835 = DIRECTION ( 'NONE',  ( -2.326004358982014616E-14, 0.5000000000030029312, -0.8660254037827048723 ) ) ;
#22836 = ADVANCED_FACE ( 'NONE', ( #9337 ), #20120, .F. ) ;
#22837 = DATE_TIME_ROLE ( 'creation_date' ) ;
#22838 = ADVANCED_FACE ( 'NONE', ( #7569 ), #1455, .T. ) ;
#22839 = DIRECTION ( 'NONE',  ( -1.000000000000000000, 2.330758767201999921E-14, 2.356218894535000080E-14 ) ) ;
#22840 = LOCAL_TIME ( 17, 37, 43.00000000000000000, #16144 ) ;
#22841 = CARTESIAN_POINT ( 'NONE',  ( 14.51399612240442671, -3581.686433941361429, 2247.717691707798622 ) ) ;
#22842 = APPROVAL_PERSON_ORGANIZATION ( #995, #21262, #12972 ) ;
#22843 = DIRECTION ( 'NONE',  ( 1.000000000000000000, 0.000000000000000000, 0.000000000000000000 ) ) ;
#22844 = CARTESIAN_POINT ( 'NONE',  ( 86.05520000000001346, -3594.099999999999909, 2261.869999999999891 ) ) ;
#22845 = EDGE_LOOP ( 'NONE', ( #18646, #9787, #19689, #4990 ) ) ;
#22846 = CARTESIAN_POINT ( 'NONE',  ( 15.74707948048999917, -3695.699999999999818, 2254.503999999999905 ) ) ;
#22847 = CIRCLE ( 'NONE', #421, 3.606800000000000228 ) ;
#22848 = CARTESIAN_POINT ( 'NONE',  ( -12.69999999999997087, -3575.727659094874525, 2247.391999999782001 ) ) ;
#22849 = ORIENTED_EDGE ( 'NONE', *, *, #18884, .T. ) ;
#22850 = CARTESIAN_POINT ( 'NONE',  ( 12.69999999999999929, -3639.502500000000055, 2264.841800000000148 ) ) ;
#22851 = CARTESIAN_POINT ( 'NONE',  ( -6.349999999999999645, -3694.938000000000102, 2229.612000000000080 ) ) ;
#22852 = VERTEX_POINT ( 'NONE', #21977 ) ;
#22853 = ORIENTED_EDGE ( 'NONE', *, *, #6732, .F. ) ;
#22854 = APPROVAL_PERSON_ORGANIZATION ( #6976, #20937, #7316 ) ;
#22855 = DIRECTION ( 'NONE',  ( 1.000000000000000000, 0.000000000000000000, 0.000000000000000000 ) ) ;
#22856 = DIRECTION ( 'NONE',  ( 3.424927947643999841E-13, 2.590196616239000129E-13, 1.000000000000000000 ) ) ;
#22857 = EDGE_LOOP ( 'NONE', ( #16154, #19734, #338, #21255 ) ) ;
#22858 = CARTESIAN_POINT ( 'NONE',  ( 137.3683132029000262, -3578.148799999999937, 2242.820000000000164 ) ) ;
#22859 = CARTESIAN_POINT ( 'NONE',  ( 139.6999999999999886, -3570.287499999999909, 2268.705139999999574 ) ) ;
#22861 = DIRECTION ( 'NONE',  ( -0.000000000000000000, -1.000000000000000000, -0.000000000000000000 ) ) ;
#22860 = AXIS2_PLACEMENT_3D ( 'NONE', #5491, #3708, #7239 ) ;
#22862 = DATE_TIME_ROLE ( 'classification_date' ) ;
#22863 = AXIS2_PLACEMENT_3D ( 'NONE', #10824, #50, #394 ) ;
#22864 = CARTESIAN_POINT ( 'NONE',  ( 12.69999999999999929, -3579.494999999999891, 2245.359999999999673 ) ) ;
#22866 = FACE_OUTER_BOUND ( 'NONE', #3197, .T. ) ;
#22865 = B_SPLINE_CURVE_WITH_KNOTS ( 'NONE', 3,
 ( #10385, #7112, #22685, #21295 ),
 .UNSPECIFIED., .F., .F.,
 ( 4, 4 ),
 ( 0.000000000000000000, 0.001021189648326963767 ),
 .UNSPECIFIED. ) ;
#22867 = DIRECTION ( 'NONE',  ( 0.000000000000000000, 0.000000000000000000, -1.000000000000000000 ) ) ;
#22868 = CARTESIAN_POINT ( 'NONE',  ( 141.9677625471535123, -3657.787406547741739, 2248.991461943488048 ) ) ;
#22869 = EDGE_CURVE ( 'NONE', #10958, #3857, #4451, .T. ) ;
#22870 = ADVANCED_FACE ( 'NONE', ( #22540 ), #6340, .T. ) ;
#22871 = ORIENTED_EDGE ( 'NONE', *, *, #10723, .T. ) ;
#22872 = DIRECTION ( 'NONE',  ( 0.000000000000000000, 0.000000000000000000, 1.000000000000000000 ) ) ;
#22873 = EDGE_LOOP ( 'NONE', ( #18978, #15012, #5089, #8718, #14978, #16805 ) ) ;
#22874 = EDGE_LOOP ( 'NONE', ( #18133, #392 ) ) ;
#22875 = EDGE_CURVE ( 'NONE', #20881, #14896, #6394, .T. ) ;
#22876 = ORIENTED_EDGE ( 'NONE', *, *, #4003, .T. ) ;
#22877 = VECTOR ( 'NONE', #11401, 1000.000000000000000 ) ;
#22878 = CIRCLE ( 'NONE', #4192, 6.349999999999855760 ) ;
#22879 = CARTESIAN_POINT ( 'NONE',  ( 57.14999999999999858, -3670.300000000000182, 2250.236800000000130 ) ) ;
#22880 = ORIENTED_EDGE ( 'NONE', *, *, #18452, .F. ) ;
#22881 = ORIENTED_EDGE ( 'NONE', *, *, #8516, .F. ) ;
#22882 = PERSON_AND_ORGANIZATION_ROLE ( 'classification_officer' ) ;
#22883 = CARTESIAN_POINT ( 'NONE',  ( 145.1609999999999729, -3579.494999999999891, 2239.390999999999622 ) ) ;
#22884 = DIRECTION ( 'NONE',  ( -1.000000000000000000, 0.000000000000000000, 0.000000000000000000 ) ) ;
#22885 = EDGE_CURVE ( 'NONE', #6235, #13538, #2578, .T. ) ;
#22886 = VERTEX_POINT ( 'NONE', #1453 ) ;
#22887 = FACE_OUTER_BOUND ( 'NONE', #1805, .T. ) ;
#22888 = EDGE_CURVE ( 'NONE', #3220, #553, #18306, .T. ) ;
#22889 = DIRECTION ( 'NONE',  ( 0.000000000000000000, 0.000000000000000000, -1.000000000000000000 ) ) ;
#22890 = DIRECTION ( 'NONE',  ( 0.000000000000000000, 0.000000000000000000, 1.000000000000000000 ) ) ;
#22891 = DIRECTION ( 'NONE',  ( 0.000000000000000000, -2.848874176402999842E-12, 1.000000000000000000 ) ) ;
#22892 = VECTOR ( 'NONE', #9204, 1000.000000000000000 ) ;
#22893 = ORIENTED_EDGE ( 'NONE', *, *, #4275, .F. ) ;
#22894 = SHAPE_DEFINITION_REPRESENTATION ( #1512, #19840 ) ;
#22895 = ORIENTED_EDGE ( 'NONE', *, *, #14329, .T. ) ;
#22896 = CARTESIAN_POINT ( 'NONE',  ( 12.69999999999999929, -3649.471999999999753, 2268.705139999999574 ) ) ;
#22897 = AXIS2_PLACEMENT_3D ( 'NONE', #12908, #21473, #16533 ) ;
#22898 = AXIS2_PLACEMENT_3D ( 'NONE', #9293, #14793, #379 ) ;
#22899 = CARTESIAN_POINT ( 'NONE',  ( 10.77847718860299864, -3581.592869849620911, 2248.182432005671672 ) ) ;
#22900 = EDGE_CURVE ( 'NONE', #10742, #16618, #21314, .T. ) ;
#22901 = CARTESIAN_POINT ( 'NONE',  ( 9.855199999999999960, -3659.504999999999654, 2272.030000000000200 ) ) ;
#22902 = ORIENTED_EDGE ( 'NONE', *, *, #2411, .T. ) ;
#22903 = ORIENTED_EDGE ( 'NONE', *, *, #918, .F. ) ;
#22904 = DIRECTION ( 'NONE',  ( -0.8660254037817188832, 0.5000000000047110094, 3.181634500920069822E-14 ) ) ;
#22905 = CARTESIAN_POINT ( 'NONE',  ( 144.5397947572051862, -3576.455561248520553, 2245.871466275620605 ) ) ;
#22906 = FACE_OUTER_BOUND ( 'NONE', #7689, .T. ) ;
#22907 = AXIS2_PLACEMENT_3D ( 'NONE', #4125, #9738, #22043 ) ;
#22908 = CARTESIAN_POINT ( 'NONE',  ( 11.58645765754818413, -3662.123185233198910, 2249.431876995093717 ) ) ;
#22909 = DIRECTION ( 'NONE',  ( 1.000000000000000000, 0.000000000000000000, 0.000000000000000000 ) ) ;
#22910 = ORIENTED_EDGE ( 'NONE', *, *, #2274, .T. ) ;
#22911 = LINE ( 'NONE', #16016, #9878 ) ;
#22912 = CIRCLE ( 'NONE', #5734, 0.7620000000000001217 ) ;
#22913 = DIRECTION ( 'NONE',  ( 0.000000000000000000, 0.000000000000000000, -1.000000000000000000 ) ) ;
#22914 = CIRCLE ( 'NONE', #21812, 0.7620000000000000107 ) ;
#22915 = CARTESIAN_POINT ( 'NONE',  ( 10.36831320285999958, -3660.851200000000063, 2242.820000000000164 ) ) ;
#22916 = CARTESIAN_POINT ( 'NONE',  ( 14.81248791361788264, -3657.599670035482177, 2248.672483178674611 ) ) ;
#22917 = DIRECTION ( 'NONE',  ( 0.000000000000000000, 0.000000000000000000, 1.000000000000000000 ) ) ;
#22918 = ORIENTED_EDGE ( 'NONE', *, *, #17863, .F. ) ;
#22919 = LINE ( 'NONE', #21068, #15069 ) ;
#22920 = VERTEX_POINT ( 'NONE', #2981 ) ;
#22921 = CARTESIAN_POINT ( 'NONE',  ( 9.849632180192781306, -3543.399485434482813, 2254.996746371144127 ) ) ;
#22923 = CIRCLE ( 'NONE', #11339, 3.606799999998994366 ) ;
#22922 = DATE_TIME_ROLE ( 'classification_date' ) ;
#22924 = DIRECTION ( 'NONE',  ( -1.000000000000000000, 0.000000000000000000, 0.000000000000000000 ) ) ;
#22925 = CARTESIAN_POINT ( 'NONE',  ( 10.18227723364999981, -3658.170723028000339, 2257.881333495000035 ) ) ;
#22926 = DIRECTION ( 'NONE',  ( 0.8660254037820785955, -0.5000000000040877302, -3.181634500919918361E-14 ) ) ;
#22927 = AXIS2_PLACEMENT_3D ( 'NONE', #844, #7782, #9648 ) ;
#22928 = PRODUCT_DEFINITION ( 'UNKNOWN', '', #8248, #1275 ) ;
#22929 = CARTESIAN_POINT ( 'NONE',  ( 17.43609829863562766, -3576.295497495339077, 2246.158273476378326 ) ) ;
#22930 = CLOSED_SHELL ( 'NONE', ( #18676, #6840, #18537, #9001, #20141, #14559, #11547, #19309, #22512, #19038, #22758, #2252, #3660, #1858, #18037, #3702, #5529, #9649, #10267, #17539, #5716, #19253, #1547, #16032, #16597, #1524 ) ) ;
#22931 = CARTESIAN_POINT ( 'NONE',  ( -12.31900000000000084, -3578.860000000000127, 2244.679313203000220 ) ) ;
#22932 = EDGE_LOOP ( 'NONE', ( #8283, #13175, #12232, #21937, #13713 ) ) ;
#22933 = CARTESIAN_POINT ( 'NONE',  ( 97.99320000000000164, -3670.300000000000182, 2259.837999999999738 ) ) ;
#22934 = EDGE_CURVE ( 'NONE', #16518, #7082, #11569, .T. ) ;
#22935 = DIRECTION ( 'NONE',  ( 0.7071067811865975328, 0.000000000000000000, -0.7071067811864976127 ) ) ;
#22936 = ORIENTED_EDGE ( 'NONE', *, *, #6216, .F. ) ;
#22937 = CARTESIAN_POINT ( 'NONE',  ( 151.1299999999999955, -3544.570000000000164, 2260.600000000000364 ) ) ;
#22938 = CARTESIAN_POINT ( 'NONE',  ( 10.29540294594043459, -3657.984965862048739, 2249.249084432865402 ) ) ;
#22939 = AXIS2_PLACEMENT_3D ( 'NONE', #18218, #14171, #7029 ) ;
#22940 = ADVANCED_FACE ( 'NONE', ( #15646 ), #8151, .T. ) ;
#22941 = AXIS2_PLACEMENT_3D ( 'NONE', #11836, #13598, #20737 ) ;
#22942 = VERTEX_POINT ( 'NONE', #8613 ) ;
#22943 = CARTESIAN_POINT ( 'NONE',  ( 139.7000000002931301, -3656.372659094888149, 2239.009999999999764 ) ) ;
#22944 = ORIENTED_EDGE ( 'NONE', *, *, #19975, .T. ) ;
#22945 = AXIS2_PLACEMENT_3D ( 'NONE', #21097, #3278, #1404 ) ;
#22946 = VERTEX_POINT ( 'NONE', #20670 ) ;
#22947 = ORIENTED_EDGE ( 'NONE', *, *, #11173, .F. ) ;
#22948 = AXIS2_PLACEMENT_3D ( 'NONE', #20854, #10179, #8435 ) ;
#22949 = CARTESIAN_POINT ( 'NONE',  ( 151.1299999999999955, -3660.140000000000327, 2244.547199999999975 ) ) ;
#22950 = APPROVAL_ROLE ( '' ) ;
#22951 = CARTESIAN_POINT ( 'NONE',  ( 145.4149999978999972, -3659.505243078000149, 2244.618209833000492 ) ) ;
#22952 = ORIENTED_EDGE ( 'NONE', *, *, #4200, .T. ) ;
#22953 = DIRECTION ( 'NONE',  ( 1.000000000000000000, 0.000000000000000000, 0.000000000000000000 ) ) ;
#22954 = PERSON_AND_ORGANIZATION_ROLE ( 'creator' ) ;
#22955 = CARTESIAN_POINT ( 'NONE',  ( 66.34479999999999222, -3644.899999999999636, 2259.837999999999738 ) ) ;
#22956 = CARTESIAN_POINT ( 'NONE',  ( 15.36332509443848160, -3580.494850336225227, 2249.720163181383214 ) ) ;
#22957 = CIRCLE ( 'NONE', #5399, 2.844800000000091700 ) ;
#22958 = DIRECTION ( 'NONE',  ( 0.000000000000000000, 0.000000000000000000, -1.000000000000000000 ) ) ;
#22959 = PRODUCT_DEFINITION ( 'UNKNOWN', '', #16119, #18380 ) ;
#22960 = LINE ( 'NONE', #7271, #20685 ) ;
#22961 = DIRECTION ( 'NONE',  ( 1.000000000000000000, 0.000000000000000000, 0.000000000000000000 ) ) ;
#22962 = ORIENTED_EDGE ( 'NONE', *, *, #15360, .F. ) ;
#22963 = DIRECTION ( 'NONE',  ( 0.000000000000000000, 0.000000000000000000, 1.000000000000000000 ) ) ;
#22964 = EDGE_CURVE ( 'NONE', #17291, #957, #18322, .T. ) ;
#22965 = ORIENTED_EDGE ( 'NONE', *, *, #2383, .F. ) ;
#22966 = DIRECTION ( 'NONE',  ( 0.000000000000000000, 0.000000000000000000, -1.000000000000000000 ) ) ;
#22967 =( BOUNDED_CURVE ( )  B_SPLINE_CURVE ( 3, ( #16590, #7234, #17157, #991 ),
 .UNSPECIFIED., .F., .F. ) 
 B_SPLINE_CURVE_WITH_KNOTS ( ( 4, 4 ),
 ( 1.570796327146205540, 3.141592653589829531 ),
 .UNSPECIFIED. ) 
 CURVE ( )  GEOMETRIC_REPRESENTATION_ITEM ( )  RATIONAL_B_SPLINE_CURVE ( ( 1.000000000000000000, 0.8047378542071605967, 0.8047378542071605967, 1.000000000000000000 ) ) 
 REPRESENTATION_ITEM ( '' )  );
#22968 = EDGE_CURVE ( 'NONE', #22999, #4050, #7861, .T. ) ;
#22969 = EDGE_CURVE ( 'NONE', #10469, #19192, #17955, .T. ) ;
#22970 = DIRECTION ( 'NONE',  ( -1.000000000000000000, 0.000000000000000000, 0.000000000000000000 ) ) ;
#22971 = ORIENTED_EDGE ( 'NONE', *, *, #19975, .F. ) ;
#22972 = EDGE_LOOP ( 'NONE', ( #3664, #20022, #3551, #19340 ) ) ;
#22973 = DIRECTION ( 'NONE',  ( -1.000000000000000000, 0.000000000000000000, 0.000000000000000000 ) ) ;
#22974 = CARTESIAN_POINT ( 'NONE',  ( 10.36831320284000135, -3598.151299999999992, 2292.781800000000203 ) ) ;
#22975 = VECTOR ( 'NONE', #18106, 1000.000000000000000 ) ;
#22976 = ORIENTED_EDGE ( 'NONE', *, *, #11815, .T. ) ;
#22977 = DIRECTION ( 'NONE',  ( 0.000000000000000000, 0.000000000000000000, -1.000000000000000000 ) ) ;
#22978 = DIRECTION ( 'NONE',  ( 0.000000000000000000, 1.000000000000000000, 0.000000000000000000 ) ) ;
#22979 = CARTESIAN_POINT ( 'NONE',  ( 14.71622237244000075, -3601.513131979999798, 2279.634029254999859 ) ) ;
#22980 = AXIS2_PLACEMENT_3D ( 'NONE', #15670, #22794, #6659 ) ;
#22981 = CARTESIAN_POINT ( 'NONE',  ( 15.74707948048999917, -3543.299999999999727, 2254.503999999999905 ) ) ;
#22982 = PERSON_AND_ORGANIZATION_ROLE ( 'design_owner' ) ;
#22983 = DIRECTION ( 'NONE',  ( -1.000000000000000000, 2.330758767201999921E-14, 2.343004830739999973E-14 ) ) ;
#22984 = CARTESIAN_POINT ( 'NONE',  ( 9.917068668310200508, -3695.517456592285271, 2255.165289491444582 ) ) ;
#22985 = CARTESIAN_POINT ( 'NONE',  ( 18.30773776737111902, -3580.597427895495912, 2245.138331176275187 ) ) ;
#22986 = EDGE_CURVE ( 'NONE', #5385, #14198, #17560, .T. ) ;
#22987 = CARTESIAN_POINT ( 'NONE',  ( 137.3365850758355009, -3657.921631524508030, 2249.173164983783863 ) ) ;
#22988 = VERTEX_POINT ( 'NONE', #4856 ) ;
#22989 = CIRCLE ( 'NONE', #12902, 0.7619999999999294005 ) ;
#22990 = DIRECTION ( 'NONE',  ( -1.968992327512000303E-12, 1.000000000000000000, -3.793660610075000646E-12 ) ) ;
#22991 = VECTOR ( 'NONE', #22188, 1000.000000000000000 ) ;
#22992 = ORIENTED_EDGE ( 'NONE', *, *, #3670, .F. ) ;
#22993 = CIRCLE ( 'NONE', #6173, 0.3809999999999647002 ) ;
#22994 = VERTEX_POINT ( 'NONE', #2871 ) ;
#22995 = ORIENTED_EDGE ( 'NONE', *, *, #14477, .F. ) ;
#22996 = EDGE_CURVE ( 'NONE', #17905, #20779, #2609, .T. ) ;
#22997 = LINE ( 'NONE', #3087, #7659 ) ;
#22998 = ORIENTED_EDGE ( 'NONE', *, *, #5271, .T. ) ;
#22999 = VERTEX_POINT ( 'NONE', #19042 ) ;
#23000 = CARTESIAN_POINT ( 'NONE',  ( 5.032662079066502869, -3543.933445094263789, 2260.481544455695257 ) ) ;
#23001 = LINE ( 'NONE', #8608, #18138 ) ;
#23002 = CARTESIAN_POINT ( 'NONE',  ( 139.7000000001000046, -3576.362659094999799, 2239.009999999999764 ) ) ;
#23003 = EDGE_CURVE ( 'NONE', #15456, #22532, #17271, .T. ) ;
#23004 = ORIENTED_EDGE ( 'NONE', *, *, #20045, .T. ) ;
#23005 = EDGE_CURVE ( 'NONE', #5300, #20612, #13087, .T. ) ;
#23006 = DIRECTION ( 'NONE',  ( 1.000000000000000000, 5.432398939370942693E-28, -2.324635735433000053E-14 ) ) ;
#23007 = FACE_BOUND ( 'NONE', #3035, .T. ) ;
#23008 = DIRECTION ( 'NONE',  ( -1.000000000000000000, 0.000000000000000000, 0.000000000000000000 ) ) ;
#23009 = VECTOR ( 'NONE', #13969, 1000.000000000000000 ) ;
#23010 = CARTESIAN_POINT ( 'NONE',  ( 12.69999999971559212, -3596.365159094870251, 2296.591799999999694 ) ) ;
#23011 = ORIENTED_EDGE ( 'NONE', *, *, #8360, .T. ) ;
#23012 = PERSON_AND_ORGANIZATION ( #5446, #1895 ) ;
#23013 = AXIS2_PLACEMENT_3D ( 'NONE', #16522, #14897, #474 ) ;
#23014 = ORIENTED_EDGE ( 'NONE', *, *, #8012, .T. ) ;
#23015 = AXIS2_PLACEMENT_3D ( 'NONE', #2272, #13266, #9420 ) ;
#23016 = CARTESIAN_POINT ( 'NONE',  ( 9.855190710340998805, -3579.506215806999990, 2250.162457373000052 ) ) ;
#23017 = EDGE_CURVE ( 'NONE', #10297, #2915, #19074, .T. ) ;
#23018 = CARTESIAN_POINT ( 'NONE',  ( 10.30632217271526407, -3581.032148460298231, 2249.229053156336704 ) ) ;
#23019 = CARTESIAN_POINT ( 'NONE',  ( -5.588000000000000078, -3544.061999999999898, 2253.487999999999829 ) ) ;
#23020 = EDGE_LOOP ( 'NONE', ( #3293, #5521, #6468, #16925 ) ) ;
#23021 = EDGE_CURVE ( 'NONE', #7518, #19268, #19836, .T. ) ;
#23022 = CARTESIAN_POINT ( 'NONE',  ( 61.26424768829000556, -3694.938000000000102, 2279.065800000000309 ) ) ;
#23023 = EDGE_CURVE ( 'NONE', #982, #11364, #16822, .T. ) ;
#23024 = CARTESIAN_POINT ( 'NONE',  ( 12.69999999999999929, -3639.502500000000055, 2296.210799999999836 ) ) ;
#23025 = CARTESIAN_POINT ( 'NONE',  ( 144.3716542413253876, -3576.201486203970035, 2246.367958886398810 ) ) ;
#23026 = FACE_OUTER_BOUND ( 'NONE', #12128, .T. ) ;
#23027 = AXIS2_PLACEMENT_3D ( 'NONE', #22360, #7968, #13703 ) ;
#23028 = CARTESIAN_POINT ( 'NONE',  ( 11.90120768189071399, -3662.235409550263739, 2249.316113763095018 ) ) ;
#23029 = ORIENTED_EDGE ( 'NONE', *, *, #15026, .T. ) ;
#23030 = CARTESIAN_POINT ( 'NONE',  ( 147.3200000001525041, -3544.490134410611063, 2260.599999999840747 ) ) ;
#23031 = AXIS2_PLACEMENT_3D ( 'NONE', #6534, #17402, #1359 ) ;
#23032 = ORIENTED_EDGE ( 'NONE', *, *, #2841, .T. ) ;
#23033 = CARTESIAN_POINT ( 'NONE',  ( 63.50000000000000000, -3594.099999999999909, 2260.600000000000364 ) ) ;
#23034 = CIRCLE ( 'NONE', #12579, 0.7619999999999294005 ) ;
#23035 = EDGE_CURVE ( 'NONE', #1541, #15774, #731, .T. ) ;
#23036 = CARTESIAN_POINT ( 'NONE',  ( 12.69999999999999929, -3589.528000000000247, 2261.593139999999948 ) ) ;
#23037 = CARTESIAN_POINT ( 'NONE',  ( 14.95882340859066417, -3657.775661874956313, 2248.974051916531153 ) ) ;
#23038 = CARTESIAN_POINT ( 'NONE',  ( 137.1569580771884489, -3694.590198011679149, 2255.766443268656985 ) ) ;
#23039 = ORIENTED_EDGE ( 'NONE', *, *, #17710, .T. ) ;
#23040 = CARTESIAN_POINT ( 'NONE',  ( 127.0000000000000000, -3578.860000000000127, 2247.392000000000280 ) ) ;
#23041 = ORIENTED_EDGE ( 'NONE', *, *, #6427, .F. ) ;
#23042 = DIRECTION ( 'NONE',  ( -1.000000000000000000, 2.318894227180000040E-14, 2.343004830739999973E-14 ) ) ;
#23043 = AXIS2_PLACEMENT_3D ( 'NONE', #5099, #7089, #22884 ) ;
#23044 = CARTESIAN_POINT ( 'NONE',  ( 10.16000000000000014, -3544.253380982895578, 2255.773999999999887 ) ) ;
#23045 = APPROVAL_ROLE ( '' ) ;
#23046 = DIRECTION ( 'NONE',  ( -1.000000000000000000, 0.000000000000000000, 0.000000000000000000 ) ) ;
#23047 = AXIS2_PLACEMENT_3D ( 'NONE', #15761, #1337, #6744 ) ;
#23048 = DIRECTION ( 'NONE',  ( 0.000000000000000000, -1.000000000000000000, 0.000000000000000000 ) ) ;
#23049 = CARTESIAN_POINT ( 'NONE',  ( 116.8400000000000034, -3544.570000000000164, 2243.277199999999993 ) ) ;
#23050 = TOROIDAL_SURFACE ( 'NONE', #7731, 1.524000000000000021, 0.7620000000000000107 ) ;
#23051 = ADVANCED_FACE ( 'NONE', ( #3563, #1927, #7321 ), #5573, .F. ) ;
#23052 = DIRECTION ( 'NONE',  ( 1.000000000000000000, 0.000000000000000000, 0.000000000000000000 ) ) ;
#23053 = CARTESIAN_POINT ( 'NONE',  ( 130.6067999999989979, -3619.500000000000000, 2239.009999999999764 ) ) ;
#23054 = CIRCLE ( 'NONE', #12965, 0.7619999999999987894 ) ;
#23055 = DIRECTION ( 'NONE',  ( 1.000000000000000000, 0.000000000000000000, 0.000000000000000000 ) ) ;
#23056 = ORIENTED_EDGE ( 'NONE', *, *, #19271, .F. ) ;
#23057 = CARTESIAN_POINT ( 'NONE',  ( 10.21049783553369217, -3580.932314744964970, 2239.009999999927913 ) ) ;
#23058 = DIRECTION ( 'NONE',  ( 0.000000000000000000, -1.000000000000000000, 0.000000000000000000 ) ) ;
#23059 = ORIENTED_EDGE ( 'NONE', *, *, #8437, .T. ) ;
#23060 = DIRECTION ( 'NONE',  ( -2.336881798971000105E-14, 0.000000000000000000, -1.000000000000000000 ) ) ;
#23061 = VERTEX_POINT ( 'NONE', #172 ) ;
#23062 = CARTESIAN_POINT ( 'NONE',  ( -12.31900000000002748, -3580.206200000138779, 2245.060313203175610 ) ) ;
#23063 = CIRCLE ( 'NONE', #22323, 2.844799999998995244 ) ;
#23064 = ORIENTED_EDGE ( 'NONE', *, *, #7004, .T. ) ;
#23065 = EDGE_LOOP ( 'NONE', ( #11970, #11905, #3975, #3060 ) ) ;
#23066 = APPLIED_PERSON_AND_ORGANIZATION_ASSIGNMENT ( #15105, #18614, ( #11243 ) ) ;
#23067 = CIRCLE ( 'NONE', #615, 2.844799999998998796 ) ;
#23068 = CARTESIAN_POINT ( 'NONE',  ( 15.41268679717000012, -3579.494999999999891, 2239.391000000000076 ) ) ;
#23069 = ORIENTED_EDGE ( 'NONE', *, *, #63, .F. ) ;
#23070 = DIRECTION ( 'NONE',  ( 1.000000000000000000, 0.000000000000000000, 0.000000000000000000 ) ) ;
#23071 = PERSON_AND_ORGANIZATION_ROLE ( 'creator' ) ;
#23072 = DIRECTION ( 'NONE',  ( 0.000000000000000000, -1.000000000000000000, 0.000000000000000000 ) ) ;
#23073 = CARTESIAN_POINT ( 'NONE',  ( 15.18361069157601229, -3580.883465275520393, 2249.392984458128922 ) ) ;
#23074 = AXIS2_PLACEMENT_3D ( 'NONE', #9143, #16509, #17809 ) ;
#23075 = CARTESIAN_POINT ( 'NONE',  ( 25.39999999999999858, -3568.700000000000273, 2259.837999999999738 ) ) ;
#23076 = CARTESIAN_POINT ( 'NONE',  ( 142.4730284656999970, -3660.140000970000074, 2250.236800000000130 ) ) ;
#23077 = AXIS2_PLACEMENT_3D ( 'NONE', #21505, #5454, #17978 ) ;
#23078 = DIRECTION ( 'NONE',  ( 0.000000000000000000, 0.000000000000000000, 1.000000000000000000 ) ) ;
#23079 = EDGE_LOOP ( 'NONE', ( #663, #20974, #13126, #11939 ) ) ;
#23080 = DIRECTION ( 'NONE',  ( -1.000000000000000000, 0.000000000000000000, 0.000000000000000000 ) ) ;
#23081 = CIRCLE ( 'NONE', #5518, 6.477000000000010971 ) ;
#23082 = ORIENTED_EDGE ( 'NONE', *, *, #22158, .F. ) ;
#23083 = DIRECTION ( 'NONE',  ( 0.000000000000000000, -1.000000000000000000, 0.000000000000000000 ) ) ;
#23084 = DIRECTION ( 'NONE',  ( 0.000000000000000000, -1.000000000000000000, 0.000000000000000000 ) ) ;
#23085 = DIRECTION ( 'NONE',  ( 0.000000000000000000, 0.000000000000000000, -1.000000000000000000 ) ) ;
#23086 = VERTEX_POINT ( 'NONE', #14475 ) ;
#23087 = CARTESIAN_POINT ( 'NONE',  ( -5.588000000000000078, -3544.061999999999898, 2229.612000000000080 ) ) ;
#23088 = DIRECTION ( 'NONE',  ( 0.000000000000000000, -1.000000000000000000, 0.000000000000000000 ) ) ;
#23089 = ORIENTED_EDGE ( 'NONE', *, *, #9430, .F. ) ;
#23090 = APPROVAL ( #14705, 'UNSPECIFIED' ) ;
#23091 = AXIS2_PLACEMENT_3D ( 'NONE', #3886, #12792, #16197 ) ;
#23092 = CARTESIAN_POINT ( 'NONE',  ( 9.855199999999999960, -3599.497499999999945, 2281.351799999999912 ) ) ;
#23093 = DIRECTION ( 'NONE',  ( 0.7249994335945011414, 0.000000000000000000, -0.6887494619146010688 ) ) ;
#23094 =( NAMED_UNIT ( * ) SI_UNIT ( $, .STERADIAN. ) SOLID_ANGLE_UNIT ( ) );
#23095 = EDGE_CURVE ( 'NONE', #18679, #11737, #11963, .T. ) ;
#23096 = DIRECTION ( 'NONE',  ( 0.000000000000000000, 0.000000000000000000, 1.000000000000000000 ) ) ;
#23097 = APPROVAL_STATUS ( 'not_yet_approved' ) ;
#23098 = ORIENTED_EDGE ( 'NONE', *, *, #9137, .F. ) ;
#23099 = ADVANCED_FACE ( 'NONE', ( #19857 ), #1866, .T. ) ;
#23100 = AXIS2_PLACEMENT_3D ( 'NONE', #16199, #14099, #3766 ) ;
#23101 = CARTESIAN_POINT ( 'NONE',  ( 137.3683132029016178, -3660.851200000195149, 2239.167815367238745 ) ) ;
#23102 = FACE_OUTER_BOUND ( 'NONE', #11755, .T. ) ;
#23104 = ADVANCED_FACE ( 'NONE', ( #3681 ), #6357, .T. ) ;
#23103 = CARTESIAN_POINT ( 'NONE',  ( 116.8400000000000034, -3694.430000000000291, 2251.506800000000112 ) ) ;
#23105 = ADVANCED_FACE ( 'NONE', ( #10831 ), #59, .F. ) ;
#23106 = CARTESIAN_POINT ( 'NONE',  ( 137.0738540380190216, -3658.411045518359970, 2249.651344139286721 ) ) ;
#23107 = ORIENTED_EDGE ( 'NONE', *, *, #10979, .F. ) ;
#23108 =( BOUNDED_CURVE ( )  B_SPLINE_CURVE ( 3, ( #19956, #11163, #18302, #14795 ),
 .UNSPECIFIED., .F., .T. ) 
 B_SPLINE_CURVE_WITH_KNOTS ( ( 4, 4 ),
 ( 1.570796327398617187, 3.141592653589748263 ),
 .UNSPECIFIED. ) 
 CURVE ( )  GEOMETRIC_REPRESENTATION_ITEM ( )  RATIONAL_B_SPLINE_CURVE ( ( 1.000000000000000000, 0.8047378542666738799, 0.8047378542666738799, 1.000000000000000000 ) ) 
 REPRESENTATION_ITEM ( '' )  );
#23109 = CARTESIAN_POINT ( 'NONE',  ( 137.1703043731272658, -3660.806955517932238, 2250.157730413952777 ) ) ;
#23110 = AXIS2_PLACEMENT_3D ( 'NONE', #19782, #10865, #1845 ) ;
#23111 = ORIENTED_EDGE ( 'NONE', *, *, #4207, .T. ) ;
#23112 = EDGE_CURVE ( 'NONE', #10464, #15794, #4850, .T. ) ;
#23113 = EDGE_LOOP ( 'NONE', ( #12092, #14201, #13949, #13487, #9179, #13909 ) ) ;
#23114 = EDGE_LOOP ( 'NONE', ( #18925, #1755, #3250 ) ) ;
#23115 = CARTESIAN_POINT ( 'NONE',  ( 134.6199999999999761, -3579.494999999999891, 2244.978999999999814 ) ) ;
#23116 = ORIENTED_EDGE ( 'NONE', *, *, #5932, .T. ) ;
#23117 = ORIENTED_EDGE ( 'NONE', *, *, #15951, .T. ) ;
#23118 = DIRECTION ( 'NONE',  ( 1.000000000000000000, 0.000000000000000000, 0.000000000000000000 ) ) ;
#23119 = EDGE_CURVE ( 'NONE', #5432, #20367, #18093, .T. ) ;
#23120 = DIRECTION ( 'NONE',  ( 0.000000000000000000, 1.000000000000000000, 0.000000000000000000 ) ) ;
#23121 = DIRECTION ( 'NONE',  ( 0.000000000000000000, 0.000000000000000000, -1.000000000000000000 ) ) ;
#23122 = EDGE_LOOP ( 'NONE', ( #13762, #4339, #1017, #2731 ) ) ;
#23123 = DIRECTION ( 'NONE',  ( 0.000000000000000000, 0.000000000000000000, -1.000000000000000000 ) ) ;
#23124 = FACE_BOUND ( 'NONE', #18983, .T. ) ;
#23125 = CARTESIAN_POINT ( 'NONE',  ( 133.2229999999989900, -3579.494999999999891, 2239.009999999999764 ) ) ;
#23126 = CARTESIAN_POINT ( 'NONE',  ( 3.048000000000000043, -3694.938000000000102, 2239.009999999999764 ) ) ;
#23127 = ORIENTED_EDGE ( 'NONE', *, *, #15959, .T. ) ;
#23128 = DATE_AND_TIME ( #5689, #10510 ) ;
#23129 = CARTESIAN_POINT ( 'NONE',  ( 131.5729205195000020, -3543.299999999999727, 2259.329999999999927 ) ) ;
#23130 = ADVANCED_FACE ( 'NONE', ( #19505 ), #5103, .T. ) ;
#23131 = DIRECTION ( 'NONE',  ( 0.000000000000000000, 0.000000000000000000, -1.000000000000000000 ) ) ;
#23132 = FACE_OUTER_BOUND ( 'NONE', #12686, .T. ) ;
#23133 = ORIENTED_EDGE ( 'NONE', *, *, #4371, .F. ) ;
#23134 = CARTESIAN_POINT ( 'NONE',  ( 53.64479999999999649, -3619.500000000000000, 2259.837999999999738 ) ) ;
#23135 = ADVANCED_FACE ( 'NONE', ( #8962, #23124, #14007, #16109, #5330, #7204, #7093, #21155, #3447, #10478, #1689, #14240, #17624, #1573, #23007, #6983, #12358, #10600, #12475, #10718, #7653, #20093, #11290, #4144, #5918, #5685, #18208 ), #18546, .T. ) ;
#23136 = DIRECTION ( 'NONE',  ( -1.000000000000000000, 0.000000000000000000, 0.000000000000000000 ) ) ;
#23137 = DIRECTION ( 'NONE',  ( 0.000000000000000000, 0.000000000000000000, -1.000000000000000000 ) ) ;
#23138 = DIRECTION ( 'NONE',  ( 1.000000000000000000, 0.000000000000000000, 0.000000000000000000 ) ) ;
#23139 = LINE ( 'NONE', #20112, #21510 ) ;
#23140 = DIRECTION ( 'NONE',  ( -1.000000000000000000, 0.000000000000000000, 0.000000000000000000 ) ) ;
#23141 = ORIENTED_EDGE ( 'NONE', *, *, #11669, .F. ) ;
#23142 = CARTESIAN_POINT ( 'NONE',  ( 139.6999999999999886, -3579.494999999999891, 2239.009999999999764 ) ) ;
#23143 = TOROIDAL_SURFACE ( 'NONE', #17529, 3.606799999998999695, 0.7620000000000000107 ) ;
#23144 = CARTESIAN_POINT ( 'NONE',  ( 50.79999999999999716, -3568.700000000000273, 2260.600000000000364 ) ) ;
#23145 = CARTESIAN_POINT ( 'NONE',  ( 7.020566483207999475, -3660.139755500999854, 2244.547200037999573 ) ) ;
#23146 = CARTESIAN_POINT ( 'NONE',  ( 14.72058396313755146, -3657.501534252188321, 2248.460308617039573 ) ) ;
#23147 = CARTESIAN_POINT ( 'NONE',  ( 136.6986431023520652, -3695.699999999999818, 2254.618513962067482 ) ) ;
#23148 = ORIENTED_EDGE ( 'NONE', *, *, #6221, .F. ) ;
#23149 = CARTESIAN_POINT ( 'NONE',  ( 10.36831320283000046, -3600.843699999999899, 2292.781800000000203 ) ) ;
#23150 = ORIENTED_EDGE ( 'NONE', *, *, #20010, .F. ) ;
#23151 = PLANE ( 'NONE',  #69 ) ;
#23152 = DIRECTION ( 'NONE',  ( 0.000000000000000000, 0.000000000000000000, -1.000000000000000000 ) ) ;
#23153 = DATE_AND_TIME ( #12395, #17238 ) ;
#23154 = LINE ( 'NONE', #2312, #6453 ) ;
#23155 = CARTESIAN_POINT ( 'NONE',  ( 114.2999999999999972, -3594.099999999999909, 2259.837999999999738 ) ) ;
#23156 = CARTESIAN_POINT ( 'NONE',  ( 137.1599999999999966, -3694.430000000000291, 2255.774000000000342 ) ) ;
#23157 = VECTOR ( 'NONE', #1725, 1000.000000000000000 ) ;
#23158 = CARTESIAN_POINT ( 'NONE',  ( 127.0000000000000000, -3568.700000000000273, 2239.771999999999935 ) ) ;
#23159 = EDGE_CURVE ( 'NONE', #21628, #1371, #13845, .T. ) ;
#23160 = EDGE_CURVE ( 'NONE', #21686, #3088, #3731, .T. ) ;
#23161 = ADVANCED_FACE ( 'NONE', ( #14928 ), #14586, .T. ) ;
#23162 = EDGE_CURVE ( 'NONE', #12135, #9973, #14700, .T. ) ;
#23163 = VERTEX_POINT ( 'NONE', #2391 ) ;
#23164 = ORIENTED_EDGE ( 'NONE', *, *, #16111, .T. ) ;
#23165 = NEXT_ASSEMBLY_USAGE_OCCURRENCE ( 'NAUO1', ' ', ' ', #17087, #15652, $ ) ;
#23166 = NEXT_ASSEMBLY_USAGE_OCCURRENCE ( 'NAUO2', ' ', ' ', #17087, #22928, $ ) ;
#23167 = NEXT_ASSEMBLY_USAGE_OCCURRENCE ( 'NAUO3', ' ', ' ', #17087, #22639, $ ) ;
#23168 = NEXT_ASSEMBLY_USAGE_OCCURRENCE ( 'NAUO4', ' ', ' ', #17087, #20503, $ ) ;
#23169 = NEXT_ASSEMBLY_USAGE_OCCURRENCE ( 'NAUO5', ' ', ' ', #17087, #1759, $ ) ;
#23170 = NEXT_ASSEMBLY_USAGE_OCCURRENCE ( 'NAUO6', ' ', ' ', #17087, #9636, $ ) ;
#23171 = NEXT_ASSEMBLY_USAGE_OCCURRENCE ( 'NAUO7', ' ', ' ', #17087, #22796, $ ) ;
#23172 = NEXT_ASSEMBLY_USAGE_OCCURRENCE ( 'NAUO8', ' ', ' ', #17087, #12365, $ ) ;
#23173 = NEXT_ASSEMBLY_USAGE_OCCURRENCE ( 'NAUO9', ' ', ' ', #17087, #12786, $ ) ;
#23174 = NEXT_ASSEMBLY_USAGE_OCCURRENCE ( 'NAUO10', ' ', ' ', #17087, #3469, $ ) ;
#23175 = NEXT_ASSEMBLY_USAGE_OCCURRENCE ( 'NAUO11', ' ', ' ', #17087, #20962, $ ) ;
#23176 = NEXT_ASSEMBLY_USAGE_OCCURRENCE ( 'NAUO12', ' ', ' ', #17087, #11226, $ ) ;
#23177 = NEXT_ASSEMBLY_USAGE_OCCURRENCE ( 'NAUO13', ' ', ' ', #17087, #5365, $ ) ;
#23178 = NEXT_ASSEMBLY_USAGE_OCCURRENCE ( 'NAUO14', ' ', ' ', #17087, #10933, $ ) ;
#23179 = NEXT_ASSEMBLY_USAGE_OCCURRENCE ( 'NAUO15', ' ', ' ', #17087, #22959, $ ) ;
#23180=COLOUR_RGB('Dark Blue',0.08,0.2,0.34);
#23181=FILL_AREA_STYLE_COLOUR('',#23180);
#23182=FILL_AREA_STYLE('',(#23181));
#23183=SURFACE_STYLE_FILL_AREA(#23182);
#23184=SURFACE_SIDE_STYLE('',(#23183));
#23185=SURFACE_STYLE_USAGE(.BOTH.,#23184);
#23186=PRESENTATION_STYLE_ASSIGNMENT((#23185));
#23187=COLOUR_RGB('Light Blue',0.38,0.62,0.78);
#23188=FILL_AREA_STYLE_COLOUR('',#23187);
#23189=FILL_AREA_STYLE('',(#23188));
#23190=SURFACE_STYLE_FILL_AREA(#23189);
#23191=SURFACE_SIDE_STYLE('',(#23190));
#23192=SURFACE_STYLE_USAGE(.BOTH.,#23191);
#23193=PRESENTATION_STYLE_ASSIGNMENT((#23192));
#23194=COLOUR_RGB('Sky Blue',0.24,0.69,0.87);
#23195=FILL_AREA_STYLE_COLOUR('',#23194);
#23196=FILL_AREA_STYLE('',(#23195));
#23197=SURFACE_STYLE_FILL_AREA(#23196);
#23198=SURFACE_SIDE_STYLE('',(#23197));
#23199=SURFACE_STYLE_USAGE(.BOTH.,#23198);
#23200=PRESENTATION_STYLE_ASSIGNMENT((#23199));
#23201=COLOUR_RGB('Grey',0.48,0.52,0.57);
#23202=FILL_AREA_STYLE_COLOUR('',#23201);
#23203=FILL_AREA_STYLE('',(#23202));
#23204=SURFACE_STYLE_FILL_AREA(#23203);
#23205=SURFACE_SIDE_STYLE('',(#23204));
#23206=SURFACE_STYLE_USAGE(.BOTH.,#23205);
#23207=PRESENTATION_STYLE_ASSIGNMENT((#23206));
#23208=COLOUR_RGB('Black',0.12,0.14,0.17);
#23209=FILL_AREA_STYLE_COLOUR('',#23208);
#23210=FILL_AREA_STYLE('',(#23209));
#23211=SURFACE_STYLE_FILL_AREA(#23210);
#23212=SURFACE_SIDE_STYLE('',(#23211));
#23213=SURFACE_STYLE_USAGE(.BOTH.,#23212);
#23214=PRESENTATION_STYLE_ASSIGNMENT((#23213));
#23215=COLOUR_RGB('Off White',0.89,0.88,0.83);
#23216=FILL_AREA_STYLE_COLOUR('',#23215);
#23217=FILL_AREA_STYLE('',(#23216));
#23218=SURFACE_STYLE_FILL_AREA(#23217);
#23219=SURFACE_SIDE_STYLE('',(#23218));
#23220=SURFACE_STYLE_USAGE(.BOTH.,#23219);
#23221=PRESENTATION_STYLE_ASSIGNMENT((#23220));
#23222=STYLED_ITEM('',(#23200),#13515);
#23223=STYLED_ITEM('',(#23214),#13798);
#23224=STYLED_ITEM('',(#23214),#13479);
#23225=STYLED_ITEM('',(#23214),#13372);
#23226=STYLED_ITEM('',(#23193),#21472);
#23227=STYLED_ITEM('',(#23214),#13560);
#23228=STYLED_ITEM('',(#23214),#13990);
#23229=STYLED_ITEM('',(#23221),#6209);
#23230=STYLED_ITEM('',(#23214),#21284);
#23231=STYLED_ITEM('',(#23193),#13285);
#23232=STYLED_ITEM('',(#23186),#21125);
#23233=STYLED_ITEM('',(#23214),#21208);
#23234=STYLED_ITEM('',(#23214),#6253);
#23235=STYLED_ITEM('',(#23193),#21083);
#23236=STYLED_ITEM('',(#23200),#5838);
#23237=MECHANICAL_DESIGN_GEOMETRIC_PRESENTATION_REPRESENTATION('',(#23222,#23223,#23224,#23225,#23226,#23227,#23228,#23229,#23230,#23231,#23232,#23233,#23234,#23235,#23236),#2257);
ENDSEC;
END-ISO-10303-21;
